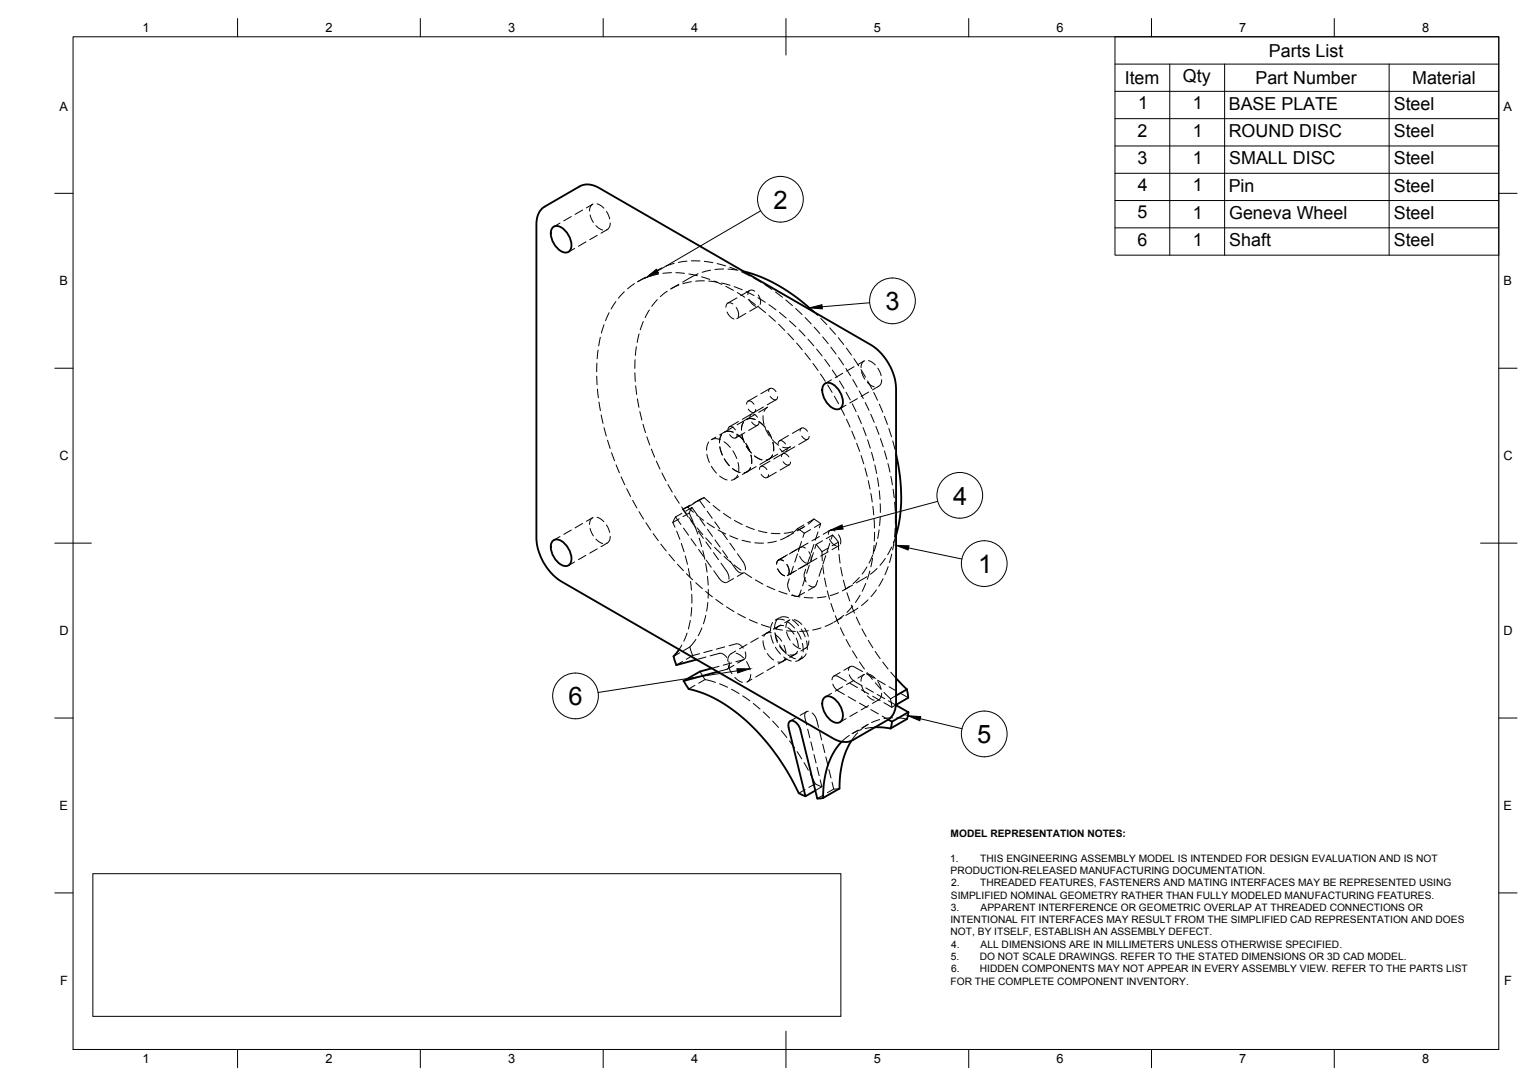
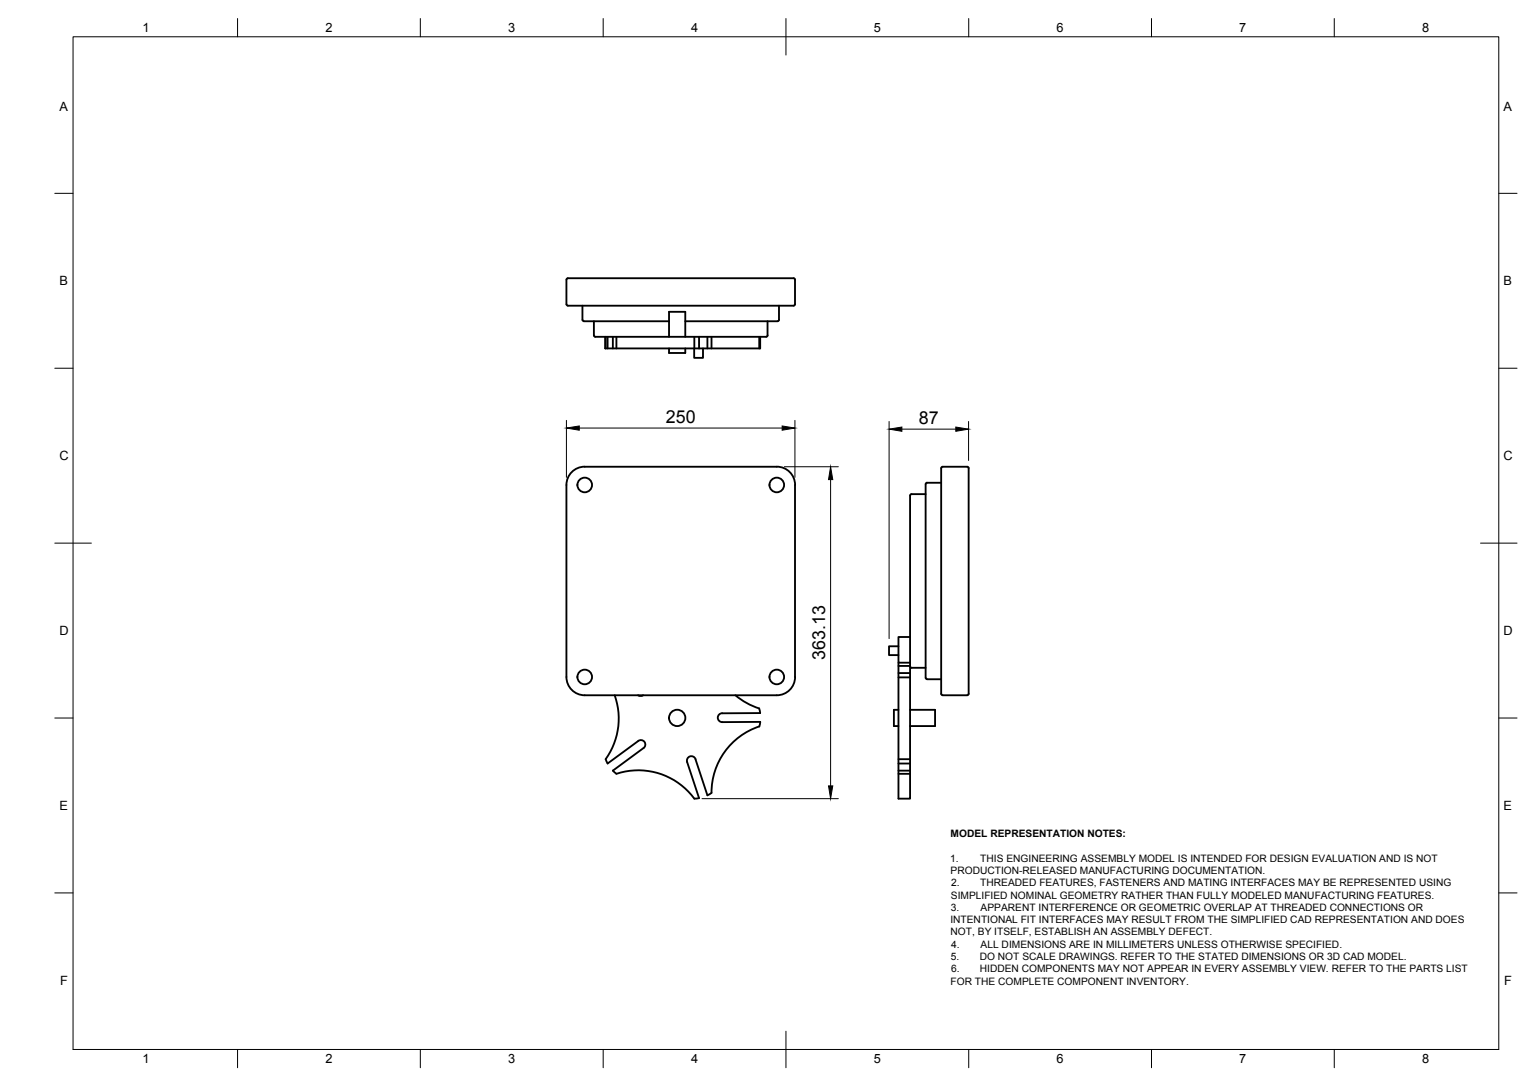
ISO-10303-21;
HEADER;
/* Generated by software containing ST-Developer
 * from STEP Tools, Inc. (www.steptools.com) 
 */

FILE_DESCRIPTION(
/* description */ ('STEP AP214'),
/* implementation_level */ '2;1');

FILE_NAME(
/* name */ 'MAS-609',
/* time_stamp */ '2026-10-06T11:20:11-07:00',
/* author */ (''),
/* organization */ (''),
/* preprocessor_version */ 'ST-DEVELOPER v20.2',
/* originating_system */ 'Autodesk Translation Framework v15.15.0.0',
/* authorisation */ '');

FILE_SCHEMA (('AUTOMOTIVE_DESIGN { 1 0 10303 214 3 1 1 }'));
ENDSEC;

DATA;
#10=MECHANICAL_DESIGN_GEOMETRIC_PRESENTATION_REPRESENTATION('',(#47,#48,
#49,#50,#51,#52),#2840);
#11=ITEM_DEFINED_TRANSFORMATION($,$,#1621,#1835);
#12=ITEM_DEFINED_TRANSFORMATION($,$,#1696,#1836);
#13=ITEM_DEFINED_TRANSFORMATION($,$,#1709,#1837);
#14=ITEM_DEFINED_TRANSFORMATION($,$,#1743,#1838);
#15=ITEM_DEFINED_TRANSFORMATION($,$,#1749,#1839);
#16=ITEM_DEFINED_TRANSFORMATION($,$,#1829,#1840);
#17=(
REPRESENTATION_RELATIONSHIP($,$,#2866,#2865)
REPRESENTATION_RELATIONSHIP_WITH_TRANSFORMATION(#11)
SHAPE_REPRESENTATION_RELATIONSHIP()
);
#18=(
REPRESENTATION_RELATIONSHIP($,$,#2867,#2865)
REPRESENTATION_RELATIONSHIP_WITH_TRANSFORMATION(#12)
SHAPE_REPRESENTATION_RELATIONSHIP()
);
#19=(
REPRESENTATION_RELATIONSHIP($,$,#2868,#2865)
REPRESENTATION_RELATIONSHIP_WITH_TRANSFORMATION(#13)
SHAPE_REPRESENTATION_RELATIONSHIP()
);
#20=(
REPRESENTATION_RELATIONSHIP($,$,#2869,#2865)
REPRESENTATION_RELATIONSHIP_WITH_TRANSFORMATION(#14)
SHAPE_REPRESENTATION_RELATIONSHIP()
);
#21=(
REPRESENTATION_RELATIONSHIP($,$,#2870,#2865)
REPRESENTATION_RELATIONSHIP_WITH_TRANSFORMATION(#15)
SHAPE_REPRESENTATION_RELATIONSHIP()
);
#22=(
REPRESENTATION_RELATIONSHIP($,$,#2871,#2865)
REPRESENTATION_RELATIONSHIP_WITH_TRANSFORMATION(#16)
SHAPE_REPRESENTATION_RELATIONSHIP()
);
#23=CONTEXT_DEPENDENT_SHAPE_REPRESENTATION(#17,#2859);
#24=CONTEXT_DEPENDENT_SHAPE_REPRESENTATION(#18,#2860);
#25=CONTEXT_DEPENDENT_SHAPE_REPRESENTATION(#19,#2861);
#26=CONTEXT_DEPENDENT_SHAPE_REPRESENTATION(#20,#2862);
#27=CONTEXT_DEPENDENT_SHAPE_REPRESENTATION(#21,#2863);
#28=CONTEXT_DEPENDENT_SHAPE_REPRESENTATION(#22,#2864);
#29=NEXT_ASSEMBLY_USAGE_OCCURRENCE('BASE PLATE:1','BASE PLATE:1',
'BASE PLATE:1',#2873,#2874,'BASE PLATE:1');
#30=NEXT_ASSEMBLY_USAGE_OCCURRENCE('ROUND DISC:1','ROUND DISC:1',
'ROUND DISC:1',#2873,#2875,'ROUND DISC:1');
#31=NEXT_ASSEMBLY_USAGE_OCCURRENCE('SMALL DISC:1','SMALL DISC:1',
'SMALL DISC:1',#2873,#2876,'SMALL DISC:1');
#32=NEXT_ASSEMBLY_USAGE_OCCURRENCE('PIN:1','PIN:1','PIN:1',#2873,#2877,
'PIN:1');
#33=NEXT_ASSEMBLY_USAGE_OCCURRENCE('Geneva Wheel:1','Geneva Wheel:1',
'Geneva Wheel:1',#2873,#2878,'Geneva Wheel:1');
#34=NEXT_ASSEMBLY_USAGE_OCCURRENCE('SHAFT:1','SHAFT:1','SHAFT:1',#2873,
#2879,'SHAFT:1');
#35=SHAPE_REPRESENTATION_RELATIONSHIP('SRR','None',#2866,#41);
#36=SHAPE_REPRESENTATION_RELATIONSHIP('SRR','None',#2867,#42);
#37=SHAPE_REPRESENTATION_RELATIONSHIP('SRR','None',#2868,#43);
#38=SHAPE_REPRESENTATION_RELATIONSHIP('SRR','None',#2869,#44);
#39=SHAPE_REPRESENTATION_RELATIONSHIP('SRR','None',#2870,#45);
#40=SHAPE_REPRESENTATION_RELATIONSHIP('SRR','None',#2871,#46);
#41=ADVANCED_BREP_SHAPE_REPRESENTATION('',(#53),#2834);
#42=ADVANCED_BREP_SHAPE_REPRESENTATION('',(#54),#2835);
#43=ADVANCED_BREP_SHAPE_REPRESENTATION('',(#55),#2836);
#44=ADVANCED_BREP_SHAPE_REPRESENTATION('',(#56),#2837);
#45=ADVANCED_BREP_SHAPE_REPRESENTATION('',(#57),#2838);
#46=ADVANCED_BREP_SHAPE_REPRESENTATION('',(#58),#2839);
#47=STYLED_ITEM('',(#2905),#53);
#48=STYLED_ITEM('',(#2905),#54);
#49=STYLED_ITEM('',(#2905),#55);
#50=STYLED_ITEM('',(#2905),#56);
#51=STYLED_ITEM('',(#2905),#57);
#52=STYLED_ITEM('',(#2905),#58);
#53=MANIFOLD_SOLID_BREP('Body1',#1547);
#54=MANIFOLD_SOLID_BREP('Body1',#1548);
#55=MANIFOLD_SOLID_BREP('Body1',#1549);
#56=MANIFOLD_SOLID_BREP('Body1',#1550);
#57=MANIFOLD_SOLID_BREP('Body1',#1551);
#58=MANIFOLD_SOLID_BREP('Body1',#1552);
#59=TOROIDAL_SURFACE('',#1663,18.5,1.5);
#60=TOROIDAL_SURFACE('',#1670,18.5,1.5);
#61=TOROIDAL_SURFACE('',#1672,18.5,1.5);
#62=TOROIDAL_SURFACE('',#1678,18.5,1.5);
#63=TOROIDAL_SURFACE('',#1679,18.5,1.5);
#64=TOROIDAL_SURFACE('',#1686,18.5,1.5);
#65=TOROIDAL_SURFACE('',#1688,18.5,1.5);
#66=TOROIDAL_SURFACE('',#1694,18.5,1.5);
#67=TOROIDAL_SURFACE('',#1700,106.,1.5);
#68=TOROIDAL_SURFACE('',#1728,13.,0.5);
#69=TOROIDAL_SURFACE('',#1734,93.5,1.5);
#70=FACE_BOUND('',#226,.T.);
#71=FACE_BOUND('',#227,.T.);
#72=FACE_BOUND('',#228,.T.);
#73=FACE_BOUND('',#229,.T.);
#74=FACE_BOUND('',#230,.T.);
#75=FACE_BOUND('',#232,.T.);
#76=FACE_BOUND('',#233,.T.);
#77=FACE_BOUND('',#234,.T.);
#78=FACE_BOUND('',#235,.T.);
#79=FACE_BOUND('',#261,.T.);
#80=FACE_BOUND('',#263,.T.);
#81=FACE_BOUND('',#275,.T.);
#82=FACE_BOUND('',#276,.T.);
#83=FACE_BOUND('',#277,.T.);
#84=FACE_BOUND('',#278,.T.);
#85=FACE_BOUND('',#279,.T.);
#86=FACE_BOUND('',#280,.T.);
#87=FACE_BOUND('',#281,.T.);
#88=FACE_BOUND('',#283,.T.);
#89=FACE_BOUND('',#284,.T.);
#90=FACE_BOUND('',#285,.T.);
#91=FACE_BOUND('',#286,.T.);
#92=FACE_BOUND('',#287,.T.);
#93=FACE_BOUND('',#288,.T.);
#94=FACE_BOUND('',#289,.T.);
#95=FACE_BOUND('',#299,.T.);
#96=FACE_BOUND('',#301,.T.);
#97=FACE_BOUND('',#330,.T.);
#98=PLANE('',#1637);
#99=PLANE('',#1638);
#100=PLANE('',#1639);
#101=PLANE('',#1640);
#102=PLANE('',#1641);
#103=PLANE('',#1646);
#104=PLANE('',#1695);
#105=PLANE('',#1707);
#106=PLANE('',#1708);
#107=PLANE('',#1741);
#108=PLANE('',#1742);
#109=PLANE('',#1747);
#110=PLANE('',#1748);
#111=PLANE('',#1765);
#112=PLANE('',#1783);
#113=PLANE('',#1802);
#114=PLANE('',#1806);
#115=PLANE('',#1808);
#116=PLANE('',#1812);
#117=PLANE('',#1813);
#118=PLANE('',#1816);
#119=PLANE('',#1817);
#120=PLANE('',#1821);
#121=PLANE('',#1823);
#122=PLANE('',#1827);
#123=PLANE('',#1828);
#124=PLANE('',#1833);
#125=PLANE('',#1834);
#126=FACE_OUTER_BOUND('',#216,.T.);
#127=FACE_OUTER_BOUND('',#217,.T.);
#128=FACE_OUTER_BOUND('',#218,.T.);
#129=FACE_OUTER_BOUND('',#219,.T.);
#130=FACE_OUTER_BOUND('',#220,.T.);
#131=FACE_OUTER_BOUND('',#221,.T.);
#132=FACE_OUTER_BOUND('',#222,.T.);
#133=FACE_OUTER_BOUND('',#223,.T.);
#134=FACE_OUTER_BOUND('',#224,.T.);
#135=FACE_OUTER_BOUND('',#225,.T.);
#136=FACE_OUTER_BOUND('',#231,.T.);
#137=FACE_OUTER_BOUND('',#236,.T.);
#138=FACE_OUTER_BOUND('',#237,.T.);
#139=FACE_OUTER_BOUND('',#238,.T.);
#140=FACE_OUTER_BOUND('',#239,.T.);
#141=FACE_OUTER_BOUND('',#240,.T.);
#142=FACE_OUTER_BOUND('',#241,.T.);
#143=FACE_OUTER_BOUND('',#242,.T.);
#144=FACE_OUTER_BOUND('',#243,.T.);
#145=FACE_OUTER_BOUND('',#244,.T.);
#146=FACE_OUTER_BOUND('',#245,.T.);
#147=FACE_OUTER_BOUND('',#246,.T.);
#148=FACE_OUTER_BOUND('',#247,.T.);
#149=FACE_OUTER_BOUND('',#248,.T.);
#150=FACE_OUTER_BOUND('',#249,.T.);
#151=FACE_OUTER_BOUND('',#250,.T.);
#152=FACE_OUTER_BOUND('',#251,.T.);
#153=FACE_OUTER_BOUND('',#252,.T.);
#154=FACE_OUTER_BOUND('',#253,.T.);
#155=FACE_OUTER_BOUND('',#254,.T.);
#156=FACE_OUTER_BOUND('',#255,.T.);
#157=FACE_OUTER_BOUND('',#256,.T.);
#158=FACE_OUTER_BOUND('',#257,.T.);
#159=FACE_OUTER_BOUND('',#258,.T.);
#160=FACE_OUTER_BOUND('',#259,.T.);
#161=FACE_OUTER_BOUND('',#260,.T.);
#162=FACE_OUTER_BOUND('',#262,.T.);
#163=FACE_OUTER_BOUND('',#264,.T.);
#164=FACE_OUTER_BOUND('',#265,.T.);
#165=FACE_OUTER_BOUND('',#266,.T.);
#166=FACE_OUTER_BOUND('',#267,.T.);
#167=FACE_OUTER_BOUND('',#268,.T.);
#168=FACE_OUTER_BOUND('',#269,.T.);
#169=FACE_OUTER_BOUND('',#270,.T.);
#170=FACE_OUTER_BOUND('',#271,.T.);
#171=FACE_OUTER_BOUND('',#272,.T.);
#172=FACE_OUTER_BOUND('',#273,.T.);
#173=FACE_OUTER_BOUND('',#274,.T.);
#174=FACE_OUTER_BOUND('',#282,.T.);
#175=FACE_OUTER_BOUND('',#290,.T.);
#176=FACE_OUTER_BOUND('',#291,.T.);
#177=FACE_OUTER_BOUND('',#292,.T.);
#178=FACE_OUTER_BOUND('',#293,.T.);
#179=FACE_OUTER_BOUND('',#294,.T.);
#180=FACE_OUTER_BOUND('',#295,.T.);
#181=FACE_OUTER_BOUND('',#296,.T.);
#182=FACE_OUTER_BOUND('',#297,.T.);
#183=FACE_OUTER_BOUND('',#298,.T.);
#184=FACE_OUTER_BOUND('',#300,.T.);
#185=FACE_OUTER_BOUND('',#302,.T.);
#186=FACE_OUTER_BOUND('',#303,.T.);
#187=FACE_OUTER_BOUND('',#304,.T.);
#188=FACE_OUTER_BOUND('',#305,.T.);
#189=FACE_OUTER_BOUND('',#306,.T.);
#190=FACE_OUTER_BOUND('',#307,.T.);
#191=FACE_OUTER_BOUND('',#308,.T.);
#192=FACE_OUTER_BOUND('',#309,.T.);
#193=FACE_OUTER_BOUND('',#310,.T.);
#194=FACE_OUTER_BOUND('',#311,.T.);
#195=FACE_OUTER_BOUND('',#312,.T.);
#196=FACE_OUTER_BOUND('',#313,.T.);
#197=FACE_OUTER_BOUND('',#314,.T.);
#198=FACE_OUTER_BOUND('',#315,.T.);
#199=FACE_OUTER_BOUND('',#316,.T.);
#200=FACE_OUTER_BOUND('',#317,.T.);
#201=FACE_OUTER_BOUND('',#318,.T.);
#202=FACE_OUTER_BOUND('',#319,.T.);
#203=FACE_OUTER_BOUND('',#320,.T.);
#204=FACE_OUTER_BOUND('',#321,.T.);
#205=FACE_OUTER_BOUND('',#322,.T.);
#206=FACE_OUTER_BOUND('',#323,.T.);
#207=FACE_OUTER_BOUND('',#324,.T.);
#208=FACE_OUTER_BOUND('',#325,.T.);
#209=FACE_OUTER_BOUND('',#326,.T.);
#210=FACE_OUTER_BOUND('',#327,.T.);
#211=FACE_OUTER_BOUND('',#328,.T.);
#212=FACE_OUTER_BOUND('',#329,.T.);
#213=FACE_OUTER_BOUND('',#331,.T.);
#214=FACE_OUTER_BOUND('',#332,.T.);
#215=FACE_OUTER_BOUND('',#333,.T.);
#216=EDGE_LOOP('',(#984,#985,#986,#987));
#217=EDGE_LOOP('',(#988,#989,#990,#991));
#218=EDGE_LOOP('',(#992,#993,#994,#995));
#219=EDGE_LOOP('',(#996,#997,#998,#999));
#220=EDGE_LOOP('',(#1000,#1001,#1002,#1003));
#221=EDGE_LOOP('',(#1004,#1005,#1006,#1007));
#222=EDGE_LOOP('',(#1008,#1009,#1010,#1011));
#223=EDGE_LOOP('',(#1012,#1013,#1014,#1015));
#224=EDGE_LOOP('',(#1016,#1017,#1018,#1019));
#225=EDGE_LOOP('',(#1020,#1021,#1022,#1023,#1024,#1025,#1026,#1027));
#226=EDGE_LOOP('',(#1028));
#227=EDGE_LOOP('',(#1029));
#228=EDGE_LOOP('',(#1030));
#229=EDGE_LOOP('',(#1031));
#230=EDGE_LOOP('',(#1032));
#231=EDGE_LOOP('',(#1033,#1034,#1035,#1036,#1037,#1038,#1039,#1040));
#232=EDGE_LOOP('',(#1041));
#233=EDGE_LOOP('',(#1042));
#234=EDGE_LOOP('',(#1043));
#235=EDGE_LOOP('',(#1044));
#236=EDGE_LOOP('',(#1045,#1046,#1047,#1048));
#237=EDGE_LOOP('',(#1049,#1050,#1051,#1052));
#238=EDGE_LOOP('',(#1053,#1054,#1055,#1056));
#239=EDGE_LOOP('',(#1057,#1058,#1059,#1060));
#240=EDGE_LOOP('',(#1061,#1062,#1063,#1064));
#241=EDGE_LOOP('',(#1065,#1066,#1067,#1068));
#242=EDGE_LOOP('',(#1069,#1070,#1071,#1072));
#243=EDGE_LOOP('',(#1073,#1074,#1075,#1076));
#244=EDGE_LOOP('',(#1077,#1078,#1079,#1080));
#245=EDGE_LOOP('',(#1081,#1082,#1083,#1084));
#246=EDGE_LOOP('',(#1085,#1086,#1087,#1088));
#247=EDGE_LOOP('',(#1089,#1090,#1091,#1092));
#248=EDGE_LOOP('',(#1093,#1094,#1095,#1096));
#249=EDGE_LOOP('',(#1097,#1098,#1099,#1100));
#250=EDGE_LOOP('',(#1101,#1102,#1103,#1104));
#251=EDGE_LOOP('',(#1105,#1106,#1107,#1108));
#252=EDGE_LOOP('',(#1109,#1110,#1111,#1112));
#253=EDGE_LOOP('',(#1113,#1114,#1115,#1116));
#254=EDGE_LOOP('',(#1117,#1118,#1119,#1120));
#255=EDGE_LOOP('',(#1121,#1122,#1123,#1124));
#256=EDGE_LOOP('',(#1125));
#257=EDGE_LOOP('',(#1126,#1127,#1128,#1129));
#258=EDGE_LOOP('',(#1130,#1131,#1132,#1133,#1134));
#259=EDGE_LOOP('',(#1135,#1136,#1137,#1138,#1139));
#260=EDGE_LOOP('',(#1140));
#261=EDGE_LOOP('',(#1141));
#262=EDGE_LOOP('',(#1142));
#263=EDGE_LOOP('',(#1143));
#264=EDGE_LOOP('',(#1144,#1145,#1146,#1147));
#265=EDGE_LOOP('',(#1148,#1149,#1150,#1151));
#266=EDGE_LOOP('',(#1152,#1153,#1154,#1155));
#267=EDGE_LOOP('',(#1156,#1157,#1158,#1159));
#268=EDGE_LOOP('',(#1160,#1161,#1162,#1163));
#269=EDGE_LOOP('',(#1164,#1165,#1166,#1167));
#270=EDGE_LOOP('',(#1168,#1169,#1170,#1171));
#271=EDGE_LOOP('',(#1172,#1173,#1174,#1175));
#272=EDGE_LOOP('',(#1176,#1177,#1178,#1179,#1180));
#273=EDGE_LOOP('',(#1181,#1182,#1183,#1184,#1185));
#274=EDGE_LOOP('',(#1186));
#275=EDGE_LOOP('',(#1187));
#276=EDGE_LOOP('',(#1188));
#277=EDGE_LOOP('',(#1189));
#278=EDGE_LOOP('',(#1190));
#279=EDGE_LOOP('',(#1191));
#280=EDGE_LOOP('',(#1192));
#281=EDGE_LOOP('',(#1193));
#282=EDGE_LOOP('',(#1194));
#283=EDGE_LOOP('',(#1195));
#284=EDGE_LOOP('',(#1196));
#285=EDGE_LOOP('',(#1197));
#286=EDGE_LOOP('',(#1198));
#287=EDGE_LOOP('',(#1199));
#288=EDGE_LOOP('',(#1200));
#289=EDGE_LOOP('',(#1201));
#290=EDGE_LOOP('',(#1202,#1203,#1204,#1205));
#291=EDGE_LOOP('',(#1206));
#292=EDGE_LOOP('',(#1207));
#293=EDGE_LOOP('',(#1208,#1209,#1210,#1211));
#294=EDGE_LOOP('',(#1212,#1213,#1214,#1215));
#295=EDGE_LOOP('',(#1216,#1217,#1218,#1219));
#296=EDGE_LOOP('',(#1220,#1221,#1222,#1223));
#297=EDGE_LOOP('',(#1224,#1225,#1226,#1227));
#298=EDGE_LOOP('',(#1228,#1229,#1230,#1231,#1232,#1233,#1234,#1235,#1236,
#1237,#1238,#1239,#1240,#1241,#1242,#1243,#1244,#1245,#1246,#1247,#1248,
#1249,#1250,#1251,#1252,#1253,#1254,#1255,#1256,#1257));
#299=EDGE_LOOP('',(#1258));
#300=EDGE_LOOP('',(#1259,#1260,#1261,#1262,#1263,#1264,#1265,#1266,#1267,
#1268,#1269,#1270,#1271,#1272,#1273,#1274,#1275,#1276,#1277,#1278,#1279,
#1280,#1281,#1282,#1283,#1284,#1285,#1286,#1287,#1288));
#301=EDGE_LOOP('',(#1289));
#302=EDGE_LOOP('',(#1290,#1291,#1292,#1293));
#303=EDGE_LOOP('',(#1294,#1295,#1296,#1297));
#304=EDGE_LOOP('',(#1298,#1299,#1300,#1301));
#305=EDGE_LOOP('',(#1302,#1303,#1304,#1305));
#306=EDGE_LOOP('',(#1306,#1307,#1308,#1309));
#307=EDGE_LOOP('',(#1310,#1311,#1312,#1313));
#308=EDGE_LOOP('',(#1314,#1315,#1316,#1317));
#309=EDGE_LOOP('',(#1318,#1319,#1320,#1321));
#310=EDGE_LOOP('',(#1322,#1323,#1324,#1325));
#311=EDGE_LOOP('',(#1326,#1327,#1328,#1329));
#312=EDGE_LOOP('',(#1330,#1331,#1332,#1333));
#313=EDGE_LOOP('',(#1334,#1335,#1336,#1337));
#314=EDGE_LOOP('',(#1338,#1339,#1340,#1341));
#315=EDGE_LOOP('',(#1342,#1343,#1344,#1345));
#316=EDGE_LOOP('',(#1346,#1347,#1348,#1349));
#317=EDGE_LOOP('',(#1350,#1351,#1352,#1353));
#318=EDGE_LOOP('',(#1354,#1355,#1356,#1357));
#319=EDGE_LOOP('',(#1358,#1359,#1360,#1361));
#320=EDGE_LOOP('',(#1362,#1363,#1364,#1365));
#321=EDGE_LOOP('',(#1366,#1367,#1368,#1369));
#322=EDGE_LOOP('',(#1370,#1371,#1372,#1373));
#323=EDGE_LOOP('',(#1374,#1375,#1376,#1377));
#324=EDGE_LOOP('',(#1378,#1379,#1380,#1381));
#325=EDGE_LOOP('',(#1382,#1383,#1384,#1385));
#326=EDGE_LOOP('',(#1386,#1387,#1388,#1389));
#327=EDGE_LOOP('',(#1390,#1391,#1392,#1393));
#328=EDGE_LOOP('',(#1394,#1395,#1396,#1397));
#329=EDGE_LOOP('',(#1398));
#330=EDGE_LOOP('',(#1399));
#331=EDGE_LOOP('',(#1400,#1401,#1402,#1403));
#332=EDGE_LOOP('',(#1404));
#333=EDGE_LOOP('',(#1405));
#334=LINE('',#2382,#427);
#335=LINE('',#2388,#428);
#336=LINE('',#2394,#429);
#337=LINE('',#2400,#430);
#338=LINE('',#2406,#431);
#339=LINE('',#2411,#432);
#340=LINE('',#2413,#433);
#341=LINE('',#2415,#434);
#342=LINE('',#2416,#435);
#343=LINE('',#2420,#436);
#344=LINE('',#2422,#437);
#345=LINE('',#2424,#438);
#346=LINE('',#2425,#439);
#347=LINE('',#2429,#440);
#348=LINE('',#2431,#441);
#349=LINE('',#2433,#442);
#350=LINE('',#2434,#443);
#351=LINE('',#2438,#444);
#352=LINE('',#2440,#445);
#353=LINE('',#2442,#446);
#354=LINE('',#2443,#447);
#355=LINE('',#2447,#448);
#356=LINE('',#2451,#449);
#357=LINE('',#2455,#450);
#358=LINE('',#2459,#451);
#359=LINE('',#2464,#452);
#360=LINE('',#2468,#453);
#361=LINE('',#2472,#454);
#362=LINE('',#2476,#455);
#363=LINE('',#2528,#456);
#364=LINE('',#2541,#457);
#365=LINE('',#2549,#458);
#366=LINE('',#2555,#459);
#367=LINE('',#2561,#460);
#368=LINE('',#2567,#461);
#369=LINE('',#2573,#462);
#370=LINE('',#2579,#463);
#371=LINE('',#2590,#464);
#372=LINE('',#2602,#465);
#373=LINE('',#2610,#466);
#374=LINE('',#2619,#467);
#375=LINE('',#2626,#468);
#376=LINE('',#2629,#469);
#377=LINE('',#2635,#470);
#378=LINE('',#2638,#471);
#379=LINE('',#2644,#472);
#380=LINE('',#2647,#473);
#381=LINE('',#2652,#474);
#382=LINE('',#2659,#475);
#383=LINE('',#2667,#476);
#384=LINE('',#2671,#477);
#385=LINE('',#2678,#478);
#386=LINE('',#2680,#479);
#387=LINE('',#2684,#480);
#388=LINE('',#2686,#481);
#389=LINE('',#2694,#482);
#390=LINE('',#2698,#483);
#391=LINE('',#2705,#484);
#392=LINE('',#2711,#485);
#393=LINE('',#2719,#486);
#394=LINE('',#2723,#487);
#395=LINE('',#2730,#488);
#396=LINE('',#2732,#489);
#397=LINE('',#2736,#490);
#398=LINE('',#2738,#491);
#399=LINE('',#2746,#492);
#400=LINE('',#2750,#493);
#401=LINE('',#2757,#494);
#402=LINE('',#2759,#495);
#403=LINE('',#2760,#496);
#404=LINE('',#2762,#497);
#405=LINE('',#2764,#498);
#406=LINE('',#2766,#499);
#407=LINE('',#2768,#500);
#408=LINE('',#2770,#501);
#409=LINE('',#2772,#502);
#410=LINE('',#2774,#503);
#411=LINE('',#2776,#504);
#412=LINE('',#2778,#505);
#413=LINE('',#2780,#506);
#414=LINE('',#2783,#507);
#415=LINE('',#2786,#508);
#416=LINE('',#2789,#509);
#417=LINE('',#2791,#510);
#418=LINE('',#2793,#511);
#419=LINE('',#2795,#512);
#420=LINE('',#2797,#513);
#421=LINE('',#2799,#514);
#422=LINE('',#2801,#515);
#423=LINE('',#2803,#516);
#424=LINE('',#2805,#517);
#425=LINE('',#2807,#518);
#426=LINE('',#2815,#519);
#427=VECTOR('',#1849,12.5000000000002);
#428=VECTOR('',#1856,8.00000000000001);
#429=VECTOR('',#1863,8.00000000000001);
#430=VECTOR('',#1870,8.00000000000001);
#431=VECTOR('',#1877,8.00000000000001);
#432=VECTOR('',#1882,1000.);
#433=VECTOR('',#1883,1000.);
#434=VECTOR('',#1884,1000.);
#435=VECTOR('',#1885,1000.);
#436=VECTOR('',#1888,1000.);
#437=VECTOR('',#1889,1000.);
#438=VECTOR('',#1890,1000.);
#439=VECTOR('',#1891,1000.);
#440=VECTOR('',#1894,1000.);
#441=VECTOR('',#1895,1000.);
#442=VECTOR('',#1896,1000.);
#443=VECTOR('',#1897,1000.);
#444=VECTOR('',#1900,1000.);
#445=VECTOR('',#1901,1000.);
#446=VECTOR('',#1902,1000.);
#447=VECTOR('',#1903,1000.);
#448=VECTOR('',#1906,1000.);
#449=VECTOR('',#1909,1000.);
#450=VECTOR('',#1912,1000.);
#451=VECTOR('',#1915,1000.);
#452=VECTOR('',#1920,1000.);
#453=VECTOR('',#1923,1000.);
#454=VECTOR('',#1926,1000.);
#455=VECTOR('',#1929,1000.);
#456=VECTOR('',#2028,12.5);
#457=VECTOR('',#2045,107.5);
#458=VECTOR('',#2056,4.92500000000001);
#459=VECTOR('',#2063,4.92500000000001);
#460=VECTOR('',#2070,3.5);
#461=VECTOR('',#2077,3.5);
#462=VECTOR('',#2084,3.5);
#463=VECTOR('',#2091,3.5);
#464=VECTOR('',#2106,12.5);
#465=VECTOR('',#2121,95.0000000000003);
#466=VECTOR('',#2132,4.83000000000002);
#467=VECTOR('',#2145,12.7);
#468=VECTOR('',#2152,1000.);
#469=VECTOR('',#2155,1000.);
#470=VECTOR('',#2160,1000.);
#471=VECTOR('',#2163,1000.);
#472=VECTOR('',#2168,1000.);
#473=VECTOR('',#2171,1000.);
#474=VECTOR('',#2176,8.88999999999999);
#475=VECTOR('',#2183,1000.);
#476=VECTOR('',#2190,1000.);
#477=VECTOR('',#2193,1000.);
#478=VECTOR('',#2200,1000.);
#479=VECTOR('',#2201,1000.);
#480=VECTOR('',#2206,1000.);
#481=VECTOR('',#2207,1000.);
#482=VECTOR('',#2214,1000.);
#483=VECTOR('',#2217,1000.);
#484=VECTOR('',#2224,1000.);
#485=VECTOR('',#2229,1000.);
#486=VECTOR('',#2236,1000.);
#487=VECTOR('',#2239,1000.);
#488=VECTOR('',#2246,1000.);
#489=VECTOR('',#2247,1000.);
#490=VECTOR('',#2252,1000.);
#491=VECTOR('',#2253,1000.);
#492=VECTOR('',#2260,1000.);
#493=VECTOR('',#2263,1000.);
#494=VECTOR('',#2270,1000.);
#495=VECTOR('',#2273,1000.);
#496=VECTOR('',#2274,1000.);
#497=VECTOR('',#2277,1000.);
#498=VECTOR('',#2280,1000.);
#499=VECTOR('',#2283,1000.);
#500=VECTOR('',#2286,1000.);
#501=VECTOR('',#2289,1000.);
#502=VECTOR('',#2292,1000.);
#503=VECTOR('',#2295,1000.);
#504=VECTOR('',#2298,1000.);
#505=VECTOR('',#2301,1000.);
#506=VECTOR('',#2304,1000.);
#507=VECTOR('',#2309,1000.);
#508=VECTOR('',#2314,1000.);
#509=VECTOR('',#2319,1000.);
#510=VECTOR('',#2322,1000.);
#511=VECTOR('',#2325,1000.);
#512=VECTOR('',#2328,1000.);
#513=VECTOR('',#2331,1000.);
#514=VECTOR('',#2334,1000.);
#515=VECTOR('',#2337,1000.);
#516=VECTOR('',#2340,1000.);
#517=VECTOR('',#2343,1000.);
#518=VECTOR('',#2346,1000.);
#519=VECTOR('',#2357,8.89);
#520=CIRCLE('',#1623,12.5000000000002);
#521=CIRCLE('',#1624,12.5000000000002);
#522=CIRCLE('',#1626,8.00000000000001);
#523=CIRCLE('',#1627,8.00000000000001);
#524=CIRCLE('',#1629,8.00000000000001);
#525=CIRCLE('',#1630,8.00000000000001);
#526=CIRCLE('',#1632,8.00000000000001);
#527=CIRCLE('',#1633,8.00000000000001);
#528=CIRCLE('',#1635,8.00000000000001);
#529=CIRCLE('',#1636,8.00000000000001);
#530=CIRCLE('',#1642,18.5);
#531=CIRCLE('',#1643,18.5);
#532=CIRCLE('',#1644,18.5);
#533=CIRCLE('',#1645,18.5);
#534=CIRCLE('',#1647,18.5);
#535=CIRCLE('',#1648,18.5);
#536=CIRCLE('',#1649,18.5);
#537=CIRCLE('',#1650,18.5);
#538=CIRCLE('',#1652,20.);
#539=CIRCLE('',#1653,20.);
#540=CIRCLE('',#1655,20.);
#541=CIRCLE('',#1656,20.);
#542=CIRCLE('',#1658,20.);
#543=CIRCLE('',#1659,20.);
#544=CIRCLE('',#1661,20.);
#545=CIRCLE('',#1662,20.);
#546=CIRCLE('',#1664,1.5);
#547=CIRCLE('',#1665,1.50000000000006);
#548=CIRCLE('',#1667,1.50000000000006);
#549=CIRCLE('',#1669,1.5);
#550=CIRCLE('',#1671,1.5);
#551=CIRCLE('',#1673,1.50000000000006);
#552=CIRCLE('',#1675,1.5);
#553=CIRCLE('',#1677,1.50000000000006);
#554=CIRCLE('',#1680,1.5);
#555=CIRCLE('',#1681,1.50000000000006);
#556=CIRCLE('',#1683,1.50000000000006);
#557=CIRCLE('',#1685,1.5);
#558=CIRCLE('',#1687,1.5);
#559=CIRCLE('',#1689,1.50000000000006);
#560=CIRCLE('',#1691,1.5);
#561=CIRCLE('',#1693,1.50000000000006);
#562=CIRCLE('',#1698,12.5);
#563=CIRCLE('',#1699,12.5);
#564=CIRCLE('',#1701,106.);
#565=CIRCLE('',#1702,1.5);
#566=CIRCLE('',#1703,107.5);
#567=CIRCLE('',#1704,107.5);
#568=CIRCLE('',#1706,107.5);
#569=CIRCLE('',#1711,4.92500000000001);
#570=CIRCLE('',#1712,4.92500000000001);
#571=CIRCLE('',#1714,4.92500000000001);
#572=CIRCLE('',#1715,4.92500000000001);
#573=CIRCLE('',#1717,3.5);
#574=CIRCLE('',#1718,3.5);
#575=CIRCLE('',#1720,3.5);
#576=CIRCLE('',#1721,3.5);
#577=CIRCLE('',#1723,3.5);
#578=CIRCLE('',#1724,3.5);
#579=CIRCLE('',#1726,3.5);
#580=CIRCLE('',#1727,3.5);
#581=CIRCLE('',#1729,12.5000000000001);
#582=CIRCLE('',#1730,0.5);
#583=CIRCLE('',#1731,13.0000000000001);
#584=CIRCLE('',#1733,12.5000000000001);
#585=CIRCLE('',#1735,93.5000000000003);
#586=CIRCLE('',#1736,1.5);
#587=CIRCLE('',#1737,95.0000000000003);
#588=CIRCLE('',#1738,95.0000000000003);
#589=CIRCLE('',#1740,95.0000000000003);
#590=CIRCLE('',#1745,4.83000000000002);
#591=CIRCLE('',#1746,4.83000000000002);
#592=CIRCLE('',#1751,12.7);
#593=CIRCLE('',#1752,12.7);
#594=CIRCLE('',#1754,4.826);
#595=CIRCLE('',#1755,4.826);
#596=CIRCLE('',#1757,76.1999999999999);
#597=CIRCLE('',#1758,76.1999999999999);
#598=CIRCLE('',#1760,4.826);
#599=CIRCLE('',#1761,4.826);
#600=CIRCLE('',#1763,8.88999999999999);
#601=CIRCLE('',#1764,8.88999999999999);
#602=CIRCLE('',#1766,4.826);
#603=CIRCLE('',#1767,27.0465001077289);
#604=CIRCLE('',#1768,76.2);
#605=CIRCLE('',#1769,27.0465001077289);
#606=CIRCLE('',#1770,4.826);
#607=CIRCLE('',#1771,27.0465001077289);
#608=CIRCLE('',#1772,76.1999999999999);
#609=CIRCLE('',#1773,27.0465001077289);
#610=CIRCLE('',#1774,27.0465001077289);
#611=CIRCLE('',#1775,27.0465001077289);
#612=CIRCLE('',#1776,27.0465001077289);
#613=CIRCLE('',#1777,76.1999999999999);
#614=CIRCLE('',#1778,27.0465001077289);
#615=CIRCLE('',#1779,4.826);
#616=CIRCLE('',#1780,27.0465001077289);
#617=CIRCLE('',#1781,76.1999999999999);
#618=CIRCLE('',#1782,27.0465001077289);
#619=CIRCLE('',#1784,4.826);
#620=CIRCLE('',#1785,27.0465001077289);
#621=CIRCLE('',#1786,76.1999999999999);
#622=CIRCLE('',#1787,27.0465001077289);
#623=CIRCLE('',#1788,4.826);
#624=CIRCLE('',#1789,27.0465001077289);
#625=CIRCLE('',#1790,76.1999999999999);
#626=CIRCLE('',#1791,27.0465001077289);
#627=CIRCLE('',#1792,27.0465001077289);
#628=CIRCLE('',#1793,27.0465001077289);
#629=CIRCLE('',#1794,27.0465001077289);
#630=CIRCLE('',#1795,76.1999999999999);
#631=CIRCLE('',#1796,27.0465001077289);
#632=CIRCLE('',#1797,4.826);
#633=CIRCLE('',#1798,27.0465001077289);
#634=CIRCLE('',#1799,76.2);
#635=CIRCLE('',#1800,27.0465001077289);
#636=CIRCLE('',#1831,8.89);
#637=CIRCLE('',#1832,8.89);
#638=VERTEX_POINT('',#2379);
#639=VERTEX_POINT('',#2381);
#640=VERTEX_POINT('',#2385);
#641=VERTEX_POINT('',#2387);
#642=VERTEX_POINT('',#2391);
#643=VERTEX_POINT('',#2393);
#644=VERTEX_POINT('',#2397);
#645=VERTEX_POINT('',#2399);
#646=VERTEX_POINT('',#2403);
#647=VERTEX_POINT('',#2405);
#648=VERTEX_POINT('',#2409);
#649=VERTEX_POINT('',#2410);
#650=VERTEX_POINT('',#2412);
#651=VERTEX_POINT('',#2414);
#652=VERTEX_POINT('',#2418);
#653=VERTEX_POINT('',#2419);
#654=VERTEX_POINT('',#2421);
#655=VERTEX_POINT('',#2423);
#656=VERTEX_POINT('',#2427);
#657=VERTEX_POINT('',#2428);
#658=VERTEX_POINT('',#2430);
#659=VERTEX_POINT('',#2432);
#660=VERTEX_POINT('',#2436);
#661=VERTEX_POINT('',#2437);
#662=VERTEX_POINT('',#2439);
#663=VERTEX_POINT('',#2441);
#664=VERTEX_POINT('',#2445);
#665=VERTEX_POINT('',#2446);
#666=VERTEX_POINT('',#2448);
#667=VERTEX_POINT('',#2450);
#668=VERTEX_POINT('',#2452);
#669=VERTEX_POINT('',#2454);
#670=VERTEX_POINT('',#2456);
#671=VERTEX_POINT('',#2458);
#672=VERTEX_POINT('',#2462);
#673=VERTEX_POINT('',#2463);
#674=VERTEX_POINT('',#2465);
#675=VERTEX_POINT('',#2467);
#676=VERTEX_POINT('',#2469);
#677=VERTEX_POINT('',#2471);
#678=VERTEX_POINT('',#2473);
#679=VERTEX_POINT('',#2475);
#680=VERTEX_POINT('',#2525);
#681=VERTEX_POINT('',#2527);
#682=VERTEX_POINT('',#2531);
#683=VERTEX_POINT('',#2533);
#684=VERTEX_POINT('',#2535);
#685=VERTEX_POINT('',#2539);
#686=VERTEX_POINT('',#2546);
#687=VERTEX_POINT('',#2548);
#688=VERTEX_POINT('',#2552);
#689=VERTEX_POINT('',#2554);
#690=VERTEX_POINT('',#2558);
#691=VERTEX_POINT('',#2560);
#692=VERTEX_POINT('',#2564);
#693=VERTEX_POINT('',#2566);
#694=VERTEX_POINT('',#2570);
#695=VERTEX_POINT('',#2572);
#696=VERTEX_POINT('',#2576);
#697=VERTEX_POINT('',#2578);
#698=VERTEX_POINT('',#2582);
#699=VERTEX_POINT('',#2584);
#700=VERTEX_POINT('',#2588);
#701=VERTEX_POINT('',#2592);
#702=VERTEX_POINT('',#2594);
#703=VERTEX_POINT('',#2596);
#704=VERTEX_POINT('',#2600);
#705=VERTEX_POINT('',#2607);
#706=VERTEX_POINT('',#2609);
#707=VERTEX_POINT('',#2616);
#708=VERTEX_POINT('',#2618);
#709=VERTEX_POINT('',#2622);
#710=VERTEX_POINT('',#2623);
#711=VERTEX_POINT('',#2625);
#712=VERTEX_POINT('',#2627);
#713=VERTEX_POINT('',#2631);
#714=VERTEX_POINT('',#2632);
#715=VERTEX_POINT('',#2634);
#716=VERTEX_POINT('',#2636);
#717=VERTEX_POINT('',#2640);
#718=VERTEX_POINT('',#2641);
#719=VERTEX_POINT('',#2643);
#720=VERTEX_POINT('',#2645);
#721=VERTEX_POINT('',#2649);
#722=VERTEX_POINT('',#2651);
#723=VERTEX_POINT('',#2655);
#724=VERTEX_POINT('',#2656);
#725=VERTEX_POINT('',#2658);
#726=VERTEX_POINT('',#2660);
#727=VERTEX_POINT('',#2662);
#728=VERTEX_POINT('',#2664);
#729=VERTEX_POINT('',#2666);
#730=VERTEX_POINT('',#2668);
#731=VERTEX_POINT('',#2670);
#732=VERTEX_POINT('',#2672);
#733=VERTEX_POINT('',#2674);
#734=VERTEX_POINT('',#2676);
#735=VERTEX_POINT('',#2679);
#736=VERTEX_POINT('',#2682);
#737=VERTEX_POINT('',#2685);
#738=VERTEX_POINT('',#2687);
#739=VERTEX_POINT('',#2689);
#740=VERTEX_POINT('',#2691);
#741=VERTEX_POINT('',#2693);
#742=VERTEX_POINT('',#2695);
#743=VERTEX_POINT('',#2697);
#744=VERTEX_POINT('',#2699);
#745=VERTEX_POINT('',#2701);
#746=VERTEX_POINT('',#2703);
#747=VERTEX_POINT('',#2707);
#748=VERTEX_POINT('',#2708);
#749=VERTEX_POINT('',#2710);
#750=VERTEX_POINT('',#2712);
#751=VERTEX_POINT('',#2714);
#752=VERTEX_POINT('',#2716);
#753=VERTEX_POINT('',#2718);
#754=VERTEX_POINT('',#2720);
#755=VERTEX_POINT('',#2722);
#756=VERTEX_POINT('',#2724);
#757=VERTEX_POINT('',#2726);
#758=VERTEX_POINT('',#2728);
#759=VERTEX_POINT('',#2731);
#760=VERTEX_POINT('',#2734);
#761=VERTEX_POINT('',#2737);
#762=VERTEX_POINT('',#2739);
#763=VERTEX_POINT('',#2741);
#764=VERTEX_POINT('',#2743);
#765=VERTEX_POINT('',#2745);
#766=VERTEX_POINT('',#2747);
#767=VERTEX_POINT('',#2749);
#768=VERTEX_POINT('',#2751);
#769=VERTEX_POINT('',#2753);
#770=VERTEX_POINT('',#2755);
#771=VERTEX_POINT('',#2812);
#772=VERTEX_POINT('',#2814);
#773=EDGE_CURVE('',#638,#638,#520,.T.);
#774=EDGE_CURVE('',#638,#639,#334,.T.);
#775=EDGE_CURVE('',#639,#639,#521,.T.);
#776=EDGE_CURVE('',#640,#640,#522,.T.);
#777=EDGE_CURVE('',#640,#641,#335,.T.);
#778=EDGE_CURVE('',#641,#641,#523,.T.);
#779=EDGE_CURVE('',#642,#642,#524,.T.);
#780=EDGE_CURVE('',#642,#643,#336,.T.);
#781=EDGE_CURVE('',#643,#643,#525,.T.);
#782=EDGE_CURVE('',#644,#644,#526,.T.);
#783=EDGE_CURVE('',#644,#645,#337,.T.);
#784=EDGE_CURVE('',#645,#645,#527,.T.);
#785=EDGE_CURVE('',#646,#646,#528,.T.);
#786=EDGE_CURVE('',#646,#647,#338,.T.);
#787=EDGE_CURVE('',#647,#647,#529,.T.);
#788=EDGE_CURVE('',#648,#649,#339,.T.);
#789=EDGE_CURVE('',#649,#650,#340,.T.);
#790=EDGE_CURVE('',#650,#651,#341,.T.);
#791=EDGE_CURVE('',#651,#648,#342,.T.);
#792=EDGE_CURVE('',#652,#653,#343,.T.);
#793=EDGE_CURVE('',#653,#654,#344,.T.);
#794=EDGE_CURVE('',#654,#655,#345,.T.);
#795=EDGE_CURVE('',#655,#652,#346,.T.);
#796=EDGE_CURVE('',#656,#657,#347,.T.);
#797=EDGE_CURVE('',#657,#658,#348,.T.);
#798=EDGE_CURVE('',#658,#659,#349,.T.);
#799=EDGE_CURVE('',#659,#656,#350,.T.);
#800=EDGE_CURVE('',#660,#661,#351,.T.);
#801=EDGE_CURVE('',#661,#662,#352,.T.);
#802=EDGE_CURVE('',#662,#663,#353,.T.);
#803=EDGE_CURVE('',#663,#660,#354,.T.);
#804=EDGE_CURVE('',#664,#665,#355,.T.);
#805=EDGE_CURVE('',#665,#666,#530,.T.);
#806=EDGE_CURVE('',#666,#667,#356,.T.);
#807=EDGE_CURVE('',#667,#668,#531,.T.);
#808=EDGE_CURVE('',#668,#669,#357,.T.);
#809=EDGE_CURVE('',#669,#670,#532,.T.);
#810=EDGE_CURVE('',#670,#671,#358,.T.);
#811=EDGE_CURVE('',#671,#664,#533,.T.);
#812=EDGE_CURVE('',#672,#673,#359,.T.);
#813=EDGE_CURVE('',#673,#674,#534,.T.);
#814=EDGE_CURVE('',#674,#675,#360,.T.);
#815=EDGE_CURVE('',#675,#676,#535,.T.);
#816=EDGE_CURVE('',#676,#677,#361,.T.);
#817=EDGE_CURVE('',#677,#678,#536,.T.);
#818=EDGE_CURVE('',#678,#679,#362,.T.);
#819=EDGE_CURVE('',#679,#672,#537,.T.);
#820=EDGE_CURVE('',#654,#657,#538,.T.);
#821=EDGE_CURVE('',#656,#655,#539,.T.);
#822=EDGE_CURVE('',#650,#653,#540,.T.);
#823=EDGE_CURVE('',#652,#651,#541,.T.);
#824=EDGE_CURVE('',#660,#649,#542,.T.);
#825=EDGE_CURVE('',#648,#661,#543,.T.);
#826=EDGE_CURVE('',#658,#663,#544,.T.);
#827=EDGE_CURVE('',#662,#659,#545,.T.);
#828=EDGE_CURVE('',#653,#677,#546,.T.);
#829=EDGE_CURVE('',#678,#650,#547,.T.);
#830=EDGE_CURVE('',#679,#649,#548,.T.);
#831=EDGE_CURVE('',#654,#676,#549,.T.);
#832=EDGE_CURVE('',#672,#660,#550,.T.);
#833=EDGE_CURVE('',#657,#675,#551,.T.);
#834=EDGE_CURVE('',#673,#663,#552,.T.);
#835=EDGE_CURVE('',#658,#674,#553,.T.);
#836=EDGE_CURVE('',#661,#669,#554,.T.);
#837=EDGE_CURVE('',#670,#648,#555,.T.);
#838=EDGE_CURVE('',#671,#651,#556,.T.);
#839=EDGE_CURVE('',#662,#668,#557,.T.);
#840=EDGE_CURVE('',#664,#652,#558,.T.);
#841=EDGE_CURVE('',#659,#667,#559,.T.);
#842=EDGE_CURVE('',#665,#655,#560,.T.);
#843=EDGE_CURVE('',#656,#666,#561,.T.);
#844=EDGE_CURVE('',#680,#680,#562,.T.);
#845=EDGE_CURVE('',#680,#681,#363,.T.);
#846=EDGE_CURVE('',#681,#681,#563,.T.);
#847=EDGE_CURVE('',#682,#682,#564,.T.);
#848=EDGE_CURVE('',#682,#683,#565,.T.);
#849=EDGE_CURVE('',#684,#683,#566,.T.);
#850=EDGE_CURVE('',#683,#684,#567,.T.);
#851=EDGE_CURVE('',#685,#685,#568,.T.);
#852=EDGE_CURVE('',#685,#684,#364,.T.);
#853=EDGE_CURVE('',#686,#686,#569,.T.);
#854=EDGE_CURVE('',#686,#687,#365,.T.);
#855=EDGE_CURVE('',#687,#687,#570,.T.);
#856=EDGE_CURVE('',#688,#688,#571,.T.);
#857=EDGE_CURVE('',#688,#689,#366,.T.);
#858=EDGE_CURVE('',#689,#689,#572,.T.);
#859=EDGE_CURVE('',#690,#690,#573,.T.);
#860=EDGE_CURVE('',#690,#691,#367,.T.);
#861=EDGE_CURVE('',#691,#691,#574,.T.);
#862=EDGE_CURVE('',#692,#692,#575,.T.);
#863=EDGE_CURVE('',#692,#693,#368,.T.);
#864=EDGE_CURVE('',#693,#693,#576,.T.);
#865=EDGE_CURVE('',#694,#694,#577,.T.);
#866=EDGE_CURVE('',#694,#695,#369,.T.);
#867=EDGE_CURVE('',#695,#695,#578,.T.);
#868=EDGE_CURVE('',#696,#696,#579,.T.);
#869=EDGE_CURVE('',#696,#697,#370,.T.);
#870=EDGE_CURVE('',#697,#697,#580,.T.);
#871=EDGE_CURVE('',#698,#698,#581,.T.);
#872=EDGE_CURVE('',#698,#699,#582,.T.);
#873=EDGE_CURVE('',#699,#699,#583,.T.);
#874=EDGE_CURVE('',#700,#700,#584,.T.);
#875=EDGE_CURVE('',#700,#698,#371,.T.);
#876=EDGE_CURVE('',#701,#701,#585,.T.);
#877=EDGE_CURVE('',#701,#702,#586,.T.);
#878=EDGE_CURVE('',#703,#702,#587,.T.);
#879=EDGE_CURVE('',#702,#703,#588,.T.);
#880=EDGE_CURVE('',#704,#704,#589,.T.);
#881=EDGE_CURVE('',#704,#703,#372,.T.);
#882=EDGE_CURVE('',#705,#705,#590,.T.);
#883=EDGE_CURVE('',#705,#706,#373,.T.);
#884=EDGE_CURVE('',#706,#706,#591,.T.);
#885=EDGE_CURVE('',#707,#707,#592,.T.);
#886=EDGE_CURVE('',#707,#708,#374,.T.);
#887=EDGE_CURVE('',#708,#708,#593,.T.);
#888=EDGE_CURVE('',#709,#710,#594,.T.);
#889=EDGE_CURVE('',#709,#711,#375,.T.);
#890=EDGE_CURVE('',#711,#712,#595,.T.);
#891=EDGE_CURVE('',#710,#712,#376,.T.);
#892=EDGE_CURVE('',#713,#714,#596,.T.);
#893=EDGE_CURVE('',#713,#715,#377,.T.);
#894=EDGE_CURVE('',#715,#716,#597,.T.);
#895=EDGE_CURVE('',#714,#716,#378,.T.);
#896=EDGE_CURVE('',#717,#718,#598,.T.);
#897=EDGE_CURVE('',#717,#719,#379,.T.);
#898=EDGE_CURVE('',#719,#720,#599,.T.);
#899=EDGE_CURVE('',#718,#720,#380,.T.);
#900=EDGE_CURVE('',#721,#721,#600,.T.);
#901=EDGE_CURVE('',#721,#722,#381,.T.);
#902=EDGE_CURVE('',#722,#722,#601,.T.);
#903=EDGE_CURVE('',#723,#724,#602,.T.);
#904=EDGE_CURVE('',#724,#725,#382,.T.);
#905=EDGE_CURVE('',#725,#726,#603,.T.);
#906=EDGE_CURVE('',#726,#727,#604,.T.);
#907=EDGE_CURVE('',#727,#728,#605,.T.);
#908=EDGE_CURVE('',#728,#729,#383,.T.);
#909=EDGE_CURVE('',#729,#730,#606,.T.);
#910=EDGE_CURVE('',#730,#731,#384,.T.);
#911=EDGE_CURVE('',#731,#732,#607,.T.);
#912=EDGE_CURVE('',#732,#733,#608,.T.);
#913=EDGE_CURVE('',#733,#734,#609,.T.);
#914=EDGE_CURVE('',#734,#717,#385,.T.);
#915=EDGE_CURVE('',#718,#735,#386,.T.);
#916=EDGE_CURVE('',#735,#713,#610,.T.);
#917=EDGE_CURVE('',#714,#736,#611,.T.);
#918=EDGE_CURVE('',#736,#709,#387,.T.);
#919=EDGE_CURVE('',#710,#737,#388,.T.);
#920=EDGE_CURVE('',#737,#738,#612,.T.);
#921=EDGE_CURVE('',#738,#739,#613,.T.);
#922=EDGE_CURVE('',#739,#740,#614,.T.);
#923=EDGE_CURVE('',#740,#741,#389,.T.);
#924=EDGE_CURVE('',#741,#742,#615,.T.);
#925=EDGE_CURVE('',#742,#743,#390,.T.);
#926=EDGE_CURVE('',#743,#744,#616,.T.);
#927=EDGE_CURVE('',#744,#745,#617,.T.);
#928=EDGE_CURVE('',#745,#746,#618,.T.);
#929=EDGE_CURVE('',#746,#723,#391,.T.);
#930=EDGE_CURVE('',#747,#748,#619,.T.);
#931=EDGE_CURVE('',#749,#747,#392,.T.);
#932=EDGE_CURVE('',#750,#749,#620,.T.);
#933=EDGE_CURVE('',#751,#750,#621,.T.);
#934=EDGE_CURVE('',#752,#751,#622,.T.);
#935=EDGE_CURVE('',#753,#752,#393,.T.);
#936=EDGE_CURVE('',#754,#753,#623,.T.);
#937=EDGE_CURVE('',#755,#754,#394,.T.);
#938=EDGE_CURVE('',#756,#755,#624,.T.);
#939=EDGE_CURVE('',#757,#756,#625,.T.);
#940=EDGE_CURVE('',#758,#757,#626,.T.);
#941=EDGE_CURVE('',#712,#758,#395,.T.);
#942=EDGE_CURVE('',#759,#711,#396,.T.);
#943=EDGE_CURVE('',#716,#759,#627,.T.);
#944=EDGE_CURVE('',#760,#715,#628,.T.);
#945=EDGE_CURVE('',#720,#760,#397,.T.);
#946=EDGE_CURVE('',#761,#719,#398,.T.);
#947=EDGE_CURVE('',#762,#761,#629,.T.);
#948=EDGE_CURVE('',#763,#762,#630,.T.);
#949=EDGE_CURVE('',#764,#763,#631,.T.);
#950=EDGE_CURVE('',#765,#764,#399,.T.);
#951=EDGE_CURVE('',#766,#765,#632,.T.);
#952=EDGE_CURVE('',#767,#766,#400,.T.);
#953=EDGE_CURVE('',#768,#767,#633,.T.);
#954=EDGE_CURVE('',#769,#768,#634,.T.);
#955=EDGE_CURVE('',#770,#769,#635,.T.);
#956=EDGE_CURVE('',#748,#770,#401,.T.);
#957=EDGE_CURVE('',#724,#748,#402,.T.);
#958=EDGE_CURVE('',#723,#747,#403,.T.);
#959=EDGE_CURVE('',#725,#770,#404,.T.);
#960=EDGE_CURVE('',#726,#769,#405,.T.);
#961=EDGE_CURVE('',#727,#768,#406,.T.);
#962=EDGE_CURVE('',#728,#767,#407,.T.);
#963=EDGE_CURVE('',#729,#766,#408,.T.);
#964=EDGE_CURVE('',#730,#765,#409,.T.);
#965=EDGE_CURVE('',#731,#764,#410,.T.);
#966=EDGE_CURVE('',#732,#763,#411,.T.);
#967=EDGE_CURVE('',#733,#762,#412,.T.);
#968=EDGE_CURVE('',#734,#761,#413,.T.);
#969=EDGE_CURVE('',#735,#760,#414,.T.);
#970=EDGE_CURVE('',#736,#759,#415,.T.);
#971=EDGE_CURVE('',#737,#758,#416,.T.);
#972=EDGE_CURVE('',#738,#757,#417,.T.);
#973=EDGE_CURVE('',#739,#756,#418,.T.);
#974=EDGE_CURVE('',#740,#755,#419,.T.);
#975=EDGE_CURVE('',#741,#754,#420,.T.);
#976=EDGE_CURVE('',#742,#753,#421,.T.);
#977=EDGE_CURVE('',#743,#752,#422,.T.);
#978=EDGE_CURVE('',#744,#751,#423,.T.);
#979=EDGE_CURVE('',#745,#750,#424,.T.);
#980=EDGE_CURVE('',#746,#749,#425,.T.);
#981=EDGE_CURVE('',#771,#771,#636,.T.);
#982=EDGE_CURVE('',#771,#772,#426,.T.);
#983=EDGE_CURVE('',#772,#772,#637,.T.);
#984=ORIENTED_EDGE('',*,*,#773,.F.);
#985=ORIENTED_EDGE('',*,*,#774,.T.);
#986=ORIENTED_EDGE('',*,*,#775,.T.);
#987=ORIENTED_EDGE('',*,*,#774,.F.);
#988=ORIENTED_EDGE('',*,*,#776,.F.);
#989=ORIENTED_EDGE('',*,*,#777,.T.);
#990=ORIENTED_EDGE('',*,*,#778,.T.);
#991=ORIENTED_EDGE('',*,*,#777,.F.);
#992=ORIENTED_EDGE('',*,*,#779,.F.);
#993=ORIENTED_EDGE('',*,*,#780,.T.);
#994=ORIENTED_EDGE('',*,*,#781,.T.);
#995=ORIENTED_EDGE('',*,*,#780,.F.);
#996=ORIENTED_EDGE('',*,*,#782,.F.);
#997=ORIENTED_EDGE('',*,*,#783,.T.);
#998=ORIENTED_EDGE('',*,*,#784,.T.);
#999=ORIENTED_EDGE('',*,*,#783,.F.);
#1000=ORIENTED_EDGE('',*,*,#785,.F.);
#1001=ORIENTED_EDGE('',*,*,#786,.T.);
#1002=ORIENTED_EDGE('',*,*,#787,.T.);
#1003=ORIENTED_EDGE('',*,*,#786,.F.);
#1004=ORIENTED_EDGE('',*,*,#788,.T.);
#1005=ORIENTED_EDGE('',*,*,#789,.T.);
#1006=ORIENTED_EDGE('',*,*,#790,.T.);
#1007=ORIENTED_EDGE('',*,*,#791,.T.);
#1008=ORIENTED_EDGE('',*,*,#792,.T.);
#1009=ORIENTED_EDGE('',*,*,#793,.T.);
#1010=ORIENTED_EDGE('',*,*,#794,.T.);
#1011=ORIENTED_EDGE('',*,*,#795,.T.);
#1012=ORIENTED_EDGE('',*,*,#796,.T.);
#1013=ORIENTED_EDGE('',*,*,#797,.T.);
#1014=ORIENTED_EDGE('',*,*,#798,.T.);
#1015=ORIENTED_EDGE('',*,*,#799,.T.);
#1016=ORIENTED_EDGE('',*,*,#800,.T.);
#1017=ORIENTED_EDGE('',*,*,#801,.T.);
#1018=ORIENTED_EDGE('',*,*,#802,.T.);
#1019=ORIENTED_EDGE('',*,*,#803,.T.);
#1020=ORIENTED_EDGE('',*,*,#804,.T.);
#1021=ORIENTED_EDGE('',*,*,#805,.T.);
#1022=ORIENTED_EDGE('',*,*,#806,.T.);
#1023=ORIENTED_EDGE('',*,*,#807,.T.);
#1024=ORIENTED_EDGE('',*,*,#808,.T.);
#1025=ORIENTED_EDGE('',*,*,#809,.T.);
#1026=ORIENTED_EDGE('',*,*,#810,.T.);
#1027=ORIENTED_EDGE('',*,*,#811,.T.);
#1028=ORIENTED_EDGE('',*,*,#778,.F.);
#1029=ORIENTED_EDGE('',*,*,#781,.F.);
#1030=ORIENTED_EDGE('',*,*,#784,.F.);
#1031=ORIENTED_EDGE('',*,*,#787,.F.);
#1032=ORIENTED_EDGE('',*,*,#775,.F.);
#1033=ORIENTED_EDGE('',*,*,#812,.T.);
#1034=ORIENTED_EDGE('',*,*,#813,.T.);
#1035=ORIENTED_EDGE('',*,*,#814,.T.);
#1036=ORIENTED_EDGE('',*,*,#815,.T.);
#1037=ORIENTED_EDGE('',*,*,#816,.T.);
#1038=ORIENTED_EDGE('',*,*,#817,.T.);
#1039=ORIENTED_EDGE('',*,*,#818,.T.);
#1040=ORIENTED_EDGE('',*,*,#819,.T.);
#1041=ORIENTED_EDGE('',*,*,#776,.T.);
#1042=ORIENTED_EDGE('',*,*,#779,.T.);
#1043=ORIENTED_EDGE('',*,*,#782,.T.);
#1044=ORIENTED_EDGE('',*,*,#785,.T.);
#1045=ORIENTED_EDGE('',*,*,#794,.F.);
#1046=ORIENTED_EDGE('',*,*,#820,.T.);
#1047=ORIENTED_EDGE('',*,*,#796,.F.);
#1048=ORIENTED_EDGE('',*,*,#821,.T.);
#1049=ORIENTED_EDGE('',*,*,#790,.F.);
#1050=ORIENTED_EDGE('',*,*,#822,.T.);
#1051=ORIENTED_EDGE('',*,*,#792,.F.);
#1052=ORIENTED_EDGE('',*,*,#823,.T.);
#1053=ORIENTED_EDGE('',*,*,#800,.F.);
#1054=ORIENTED_EDGE('',*,*,#824,.T.);
#1055=ORIENTED_EDGE('',*,*,#788,.F.);
#1056=ORIENTED_EDGE('',*,*,#825,.T.);
#1057=ORIENTED_EDGE('',*,*,#798,.F.);
#1058=ORIENTED_EDGE('',*,*,#826,.T.);
#1059=ORIENTED_EDGE('',*,*,#802,.F.);
#1060=ORIENTED_EDGE('',*,*,#827,.T.);
#1061=ORIENTED_EDGE('',*,*,#828,.F.);
#1062=ORIENTED_EDGE('',*,*,#822,.F.);
#1063=ORIENTED_EDGE('',*,*,#829,.F.);
#1064=ORIENTED_EDGE('',*,*,#817,.F.);
#1065=ORIENTED_EDGE('',*,*,#829,.T.);
#1066=ORIENTED_EDGE('',*,*,#789,.F.);
#1067=ORIENTED_EDGE('',*,*,#830,.F.);
#1068=ORIENTED_EDGE('',*,*,#818,.F.);
#1069=ORIENTED_EDGE('',*,*,#828,.T.);
#1070=ORIENTED_EDGE('',*,*,#816,.F.);
#1071=ORIENTED_EDGE('',*,*,#831,.F.);
#1072=ORIENTED_EDGE('',*,*,#793,.F.);
#1073=ORIENTED_EDGE('',*,*,#830,.T.);
#1074=ORIENTED_EDGE('',*,*,#824,.F.);
#1075=ORIENTED_EDGE('',*,*,#832,.F.);
#1076=ORIENTED_EDGE('',*,*,#819,.F.);
#1077=ORIENTED_EDGE('',*,*,#831,.T.);
#1078=ORIENTED_EDGE('',*,*,#815,.F.);
#1079=ORIENTED_EDGE('',*,*,#833,.F.);
#1080=ORIENTED_EDGE('',*,*,#820,.F.);
#1081=ORIENTED_EDGE('',*,*,#832,.T.);
#1082=ORIENTED_EDGE('',*,*,#803,.F.);
#1083=ORIENTED_EDGE('',*,*,#834,.F.);
#1084=ORIENTED_EDGE('',*,*,#812,.F.);
#1085=ORIENTED_EDGE('',*,*,#833,.T.);
#1086=ORIENTED_EDGE('',*,*,#814,.F.);
#1087=ORIENTED_EDGE('',*,*,#835,.F.);
#1088=ORIENTED_EDGE('',*,*,#797,.F.);
#1089=ORIENTED_EDGE('',*,*,#834,.T.);
#1090=ORIENTED_EDGE('',*,*,#826,.F.);
#1091=ORIENTED_EDGE('',*,*,#835,.T.);
#1092=ORIENTED_EDGE('',*,*,#813,.F.);
#1093=ORIENTED_EDGE('',*,*,#836,.F.);
#1094=ORIENTED_EDGE('',*,*,#825,.F.);
#1095=ORIENTED_EDGE('',*,*,#837,.F.);
#1096=ORIENTED_EDGE('',*,*,#809,.F.);
#1097=ORIENTED_EDGE('',*,*,#837,.T.);
#1098=ORIENTED_EDGE('',*,*,#791,.F.);
#1099=ORIENTED_EDGE('',*,*,#838,.F.);
#1100=ORIENTED_EDGE('',*,*,#810,.F.);
#1101=ORIENTED_EDGE('',*,*,#836,.T.);
#1102=ORIENTED_EDGE('',*,*,#808,.F.);
#1103=ORIENTED_EDGE('',*,*,#839,.F.);
#1104=ORIENTED_EDGE('',*,*,#801,.F.);
#1105=ORIENTED_EDGE('',*,*,#838,.T.);
#1106=ORIENTED_EDGE('',*,*,#823,.F.);
#1107=ORIENTED_EDGE('',*,*,#840,.F.);
#1108=ORIENTED_EDGE('',*,*,#811,.F.);
#1109=ORIENTED_EDGE('',*,*,#839,.T.);
#1110=ORIENTED_EDGE('',*,*,#807,.F.);
#1111=ORIENTED_EDGE('',*,*,#841,.F.);
#1112=ORIENTED_EDGE('',*,*,#827,.F.);
#1113=ORIENTED_EDGE('',*,*,#840,.T.);
#1114=ORIENTED_EDGE('',*,*,#795,.F.);
#1115=ORIENTED_EDGE('',*,*,#842,.F.);
#1116=ORIENTED_EDGE('',*,*,#804,.F.);
#1117=ORIENTED_EDGE('',*,*,#841,.T.);
#1118=ORIENTED_EDGE('',*,*,#806,.F.);
#1119=ORIENTED_EDGE('',*,*,#843,.F.);
#1120=ORIENTED_EDGE('',*,*,#799,.F.);
#1121=ORIENTED_EDGE('',*,*,#842,.T.);
#1122=ORIENTED_EDGE('',*,*,#821,.F.);
#1123=ORIENTED_EDGE('',*,*,#843,.T.);
#1124=ORIENTED_EDGE('',*,*,#805,.F.);
#1125=ORIENTED_EDGE('',*,*,#773,.T.);
#1126=ORIENTED_EDGE('',*,*,#844,.F.);
#1127=ORIENTED_EDGE('',*,*,#845,.T.);
#1128=ORIENTED_EDGE('',*,*,#846,.T.);
#1129=ORIENTED_EDGE('',*,*,#845,.F.);
#1130=ORIENTED_EDGE('',*,*,#847,.F.);
#1131=ORIENTED_EDGE('',*,*,#848,.T.);
#1132=ORIENTED_EDGE('',*,*,#849,.F.);
#1133=ORIENTED_EDGE('',*,*,#850,.F.);
#1134=ORIENTED_EDGE('',*,*,#848,.F.);
#1135=ORIENTED_EDGE('',*,*,#851,.T.);
#1136=ORIENTED_EDGE('',*,*,#852,.T.);
#1137=ORIENTED_EDGE('',*,*,#849,.T.);
#1138=ORIENTED_EDGE('',*,*,#850,.T.);
#1139=ORIENTED_EDGE('',*,*,#852,.F.);
#1140=ORIENTED_EDGE('',*,*,#847,.T.);
#1141=ORIENTED_EDGE('',*,*,#846,.F.);
#1142=ORIENTED_EDGE('',*,*,#851,.F.);
#1143=ORIENTED_EDGE('',*,*,#844,.T.);
#1144=ORIENTED_EDGE('',*,*,#853,.F.);
#1145=ORIENTED_EDGE('',*,*,#854,.T.);
#1146=ORIENTED_EDGE('',*,*,#855,.T.);
#1147=ORIENTED_EDGE('',*,*,#854,.F.);
#1148=ORIENTED_EDGE('',*,*,#856,.F.);
#1149=ORIENTED_EDGE('',*,*,#857,.T.);
#1150=ORIENTED_EDGE('',*,*,#858,.T.);
#1151=ORIENTED_EDGE('',*,*,#857,.F.);
#1152=ORIENTED_EDGE('',*,*,#859,.F.);
#1153=ORIENTED_EDGE('',*,*,#860,.T.);
#1154=ORIENTED_EDGE('',*,*,#861,.T.);
#1155=ORIENTED_EDGE('',*,*,#860,.F.);
#1156=ORIENTED_EDGE('',*,*,#862,.F.);
#1157=ORIENTED_EDGE('',*,*,#863,.T.);
#1158=ORIENTED_EDGE('',*,*,#864,.T.);
#1159=ORIENTED_EDGE('',*,*,#863,.F.);
#1160=ORIENTED_EDGE('',*,*,#865,.F.);
#1161=ORIENTED_EDGE('',*,*,#866,.T.);
#1162=ORIENTED_EDGE('',*,*,#867,.T.);
#1163=ORIENTED_EDGE('',*,*,#866,.F.);
#1164=ORIENTED_EDGE('',*,*,#868,.F.);
#1165=ORIENTED_EDGE('',*,*,#869,.T.);
#1166=ORIENTED_EDGE('',*,*,#870,.T.);
#1167=ORIENTED_EDGE('',*,*,#869,.F.);
#1168=ORIENTED_EDGE('',*,*,#871,.F.);
#1169=ORIENTED_EDGE('',*,*,#872,.T.);
#1170=ORIENTED_EDGE('',*,*,#873,.F.);
#1171=ORIENTED_EDGE('',*,*,#872,.F.);
#1172=ORIENTED_EDGE('',*,*,#874,.F.);
#1173=ORIENTED_EDGE('',*,*,#875,.T.);
#1174=ORIENTED_EDGE('',*,*,#871,.T.);
#1175=ORIENTED_EDGE('',*,*,#875,.F.);
#1176=ORIENTED_EDGE('',*,*,#876,.F.);
#1177=ORIENTED_EDGE('',*,*,#877,.T.);
#1178=ORIENTED_EDGE('',*,*,#878,.F.);
#1179=ORIENTED_EDGE('',*,*,#879,.F.);
#1180=ORIENTED_EDGE('',*,*,#877,.F.);
#1181=ORIENTED_EDGE('',*,*,#880,.T.);
#1182=ORIENTED_EDGE('',*,*,#881,.T.);
#1183=ORIENTED_EDGE('',*,*,#878,.T.);
#1184=ORIENTED_EDGE('',*,*,#879,.T.);
#1185=ORIENTED_EDGE('',*,*,#881,.F.);
#1186=ORIENTED_EDGE('',*,*,#876,.T.);
#1187=ORIENTED_EDGE('',*,*,#855,.F.);
#1188=ORIENTED_EDGE('',*,*,#858,.F.);
#1189=ORIENTED_EDGE('',*,*,#861,.F.);
#1190=ORIENTED_EDGE('',*,*,#864,.F.);
#1191=ORIENTED_EDGE('',*,*,#867,.F.);
#1192=ORIENTED_EDGE('',*,*,#870,.F.);
#1193=ORIENTED_EDGE('',*,*,#873,.T.);
#1194=ORIENTED_EDGE('',*,*,#880,.F.);
#1195=ORIENTED_EDGE('',*,*,#853,.T.);
#1196=ORIENTED_EDGE('',*,*,#856,.T.);
#1197=ORIENTED_EDGE('',*,*,#859,.T.);
#1198=ORIENTED_EDGE('',*,*,#862,.T.);
#1199=ORIENTED_EDGE('',*,*,#865,.T.);
#1200=ORIENTED_EDGE('',*,*,#868,.T.);
#1201=ORIENTED_EDGE('',*,*,#874,.T.);
#1202=ORIENTED_EDGE('',*,*,#882,.T.);
#1203=ORIENTED_EDGE('',*,*,#883,.T.);
#1204=ORIENTED_EDGE('',*,*,#884,.F.);
#1205=ORIENTED_EDGE('',*,*,#883,.F.);
#1206=ORIENTED_EDGE('',*,*,#884,.T.);
#1207=ORIENTED_EDGE('',*,*,#882,.F.);
#1208=ORIENTED_EDGE('',*,*,#885,.F.);
#1209=ORIENTED_EDGE('',*,*,#886,.T.);
#1210=ORIENTED_EDGE('',*,*,#887,.T.);
#1211=ORIENTED_EDGE('',*,*,#886,.F.);
#1212=ORIENTED_EDGE('',*,*,#888,.F.);
#1213=ORIENTED_EDGE('',*,*,#889,.T.);
#1214=ORIENTED_EDGE('',*,*,#890,.T.);
#1215=ORIENTED_EDGE('',*,*,#891,.F.);
#1216=ORIENTED_EDGE('',*,*,#892,.F.);
#1217=ORIENTED_EDGE('',*,*,#893,.T.);
#1218=ORIENTED_EDGE('',*,*,#894,.T.);
#1219=ORIENTED_EDGE('',*,*,#895,.F.);
#1220=ORIENTED_EDGE('',*,*,#896,.F.);
#1221=ORIENTED_EDGE('',*,*,#897,.T.);
#1222=ORIENTED_EDGE('',*,*,#898,.T.);
#1223=ORIENTED_EDGE('',*,*,#899,.F.);
#1224=ORIENTED_EDGE('',*,*,#900,.F.);
#1225=ORIENTED_EDGE('',*,*,#901,.T.);
#1226=ORIENTED_EDGE('',*,*,#902,.T.);
#1227=ORIENTED_EDGE('',*,*,#901,.F.);
#1228=ORIENTED_EDGE('',*,*,#903,.T.);
#1229=ORIENTED_EDGE('',*,*,#904,.T.);
#1230=ORIENTED_EDGE('',*,*,#905,.T.);
#1231=ORIENTED_EDGE('',*,*,#906,.T.);
#1232=ORIENTED_EDGE('',*,*,#907,.T.);
#1233=ORIENTED_EDGE('',*,*,#908,.T.);
#1234=ORIENTED_EDGE('',*,*,#909,.T.);
#1235=ORIENTED_EDGE('',*,*,#910,.T.);
#1236=ORIENTED_EDGE('',*,*,#911,.T.);
#1237=ORIENTED_EDGE('',*,*,#912,.T.);
#1238=ORIENTED_EDGE('',*,*,#913,.T.);
#1239=ORIENTED_EDGE('',*,*,#914,.T.);
#1240=ORIENTED_EDGE('',*,*,#896,.T.);
#1241=ORIENTED_EDGE('',*,*,#915,.T.);
#1242=ORIENTED_EDGE('',*,*,#916,.T.);
#1243=ORIENTED_EDGE('',*,*,#892,.T.);
#1244=ORIENTED_EDGE('',*,*,#917,.T.);
#1245=ORIENTED_EDGE('',*,*,#918,.T.);
#1246=ORIENTED_EDGE('',*,*,#888,.T.);
#1247=ORIENTED_EDGE('',*,*,#919,.T.);
#1248=ORIENTED_EDGE('',*,*,#920,.T.);
#1249=ORIENTED_EDGE('',*,*,#921,.T.);
#1250=ORIENTED_EDGE('',*,*,#922,.T.);
#1251=ORIENTED_EDGE('',*,*,#923,.T.);
#1252=ORIENTED_EDGE('',*,*,#924,.T.);
#1253=ORIENTED_EDGE('',*,*,#925,.T.);
#1254=ORIENTED_EDGE('',*,*,#926,.T.);
#1255=ORIENTED_EDGE('',*,*,#927,.T.);
#1256=ORIENTED_EDGE('',*,*,#928,.T.);
#1257=ORIENTED_EDGE('',*,*,#929,.T.);
#1258=ORIENTED_EDGE('',*,*,#887,.F.);
#1259=ORIENTED_EDGE('',*,*,#930,.F.);
#1260=ORIENTED_EDGE('',*,*,#931,.F.);
#1261=ORIENTED_EDGE('',*,*,#932,.F.);
#1262=ORIENTED_EDGE('',*,*,#933,.F.);
#1263=ORIENTED_EDGE('',*,*,#934,.F.);
#1264=ORIENTED_EDGE('',*,*,#935,.F.);
#1265=ORIENTED_EDGE('',*,*,#936,.F.);
#1266=ORIENTED_EDGE('',*,*,#937,.F.);
#1267=ORIENTED_EDGE('',*,*,#938,.F.);
#1268=ORIENTED_EDGE('',*,*,#939,.F.);
#1269=ORIENTED_EDGE('',*,*,#940,.F.);
#1270=ORIENTED_EDGE('',*,*,#941,.F.);
#1271=ORIENTED_EDGE('',*,*,#890,.F.);
#1272=ORIENTED_EDGE('',*,*,#942,.F.);
#1273=ORIENTED_EDGE('',*,*,#943,.F.);
#1274=ORIENTED_EDGE('',*,*,#894,.F.);
#1275=ORIENTED_EDGE('',*,*,#944,.F.);
#1276=ORIENTED_EDGE('',*,*,#945,.F.);
#1277=ORIENTED_EDGE('',*,*,#898,.F.);
#1278=ORIENTED_EDGE('',*,*,#946,.F.);
#1279=ORIENTED_EDGE('',*,*,#947,.F.);
#1280=ORIENTED_EDGE('',*,*,#948,.F.);
#1281=ORIENTED_EDGE('',*,*,#949,.F.);
#1282=ORIENTED_EDGE('',*,*,#950,.F.);
#1283=ORIENTED_EDGE('',*,*,#951,.F.);
#1284=ORIENTED_EDGE('',*,*,#952,.F.);
#1285=ORIENTED_EDGE('',*,*,#953,.F.);
#1286=ORIENTED_EDGE('',*,*,#954,.F.);
#1287=ORIENTED_EDGE('',*,*,#955,.F.);
#1288=ORIENTED_EDGE('',*,*,#956,.F.);
#1289=ORIENTED_EDGE('',*,*,#902,.F.);
#1290=ORIENTED_EDGE('',*,*,#930,.T.);
#1291=ORIENTED_EDGE('',*,*,#957,.F.);
#1292=ORIENTED_EDGE('',*,*,#903,.F.);
#1293=ORIENTED_EDGE('',*,*,#958,.T.);
#1294=ORIENTED_EDGE('',*,*,#956,.T.);
#1295=ORIENTED_EDGE('',*,*,#959,.F.);
#1296=ORIENTED_EDGE('',*,*,#904,.F.);
#1297=ORIENTED_EDGE('',*,*,#957,.T.);
#1298=ORIENTED_EDGE('',*,*,#955,.T.);
#1299=ORIENTED_EDGE('',*,*,#960,.F.);
#1300=ORIENTED_EDGE('',*,*,#905,.F.);
#1301=ORIENTED_EDGE('',*,*,#959,.T.);
#1302=ORIENTED_EDGE('',*,*,#954,.T.);
#1303=ORIENTED_EDGE('',*,*,#961,.F.);
#1304=ORIENTED_EDGE('',*,*,#906,.F.);
#1305=ORIENTED_EDGE('',*,*,#960,.T.);
#1306=ORIENTED_EDGE('',*,*,#953,.T.);
#1307=ORIENTED_EDGE('',*,*,#962,.F.);
#1308=ORIENTED_EDGE('',*,*,#907,.F.);
#1309=ORIENTED_EDGE('',*,*,#961,.T.);
#1310=ORIENTED_EDGE('',*,*,#952,.T.);
#1311=ORIENTED_EDGE('',*,*,#963,.F.);
#1312=ORIENTED_EDGE('',*,*,#908,.F.);
#1313=ORIENTED_EDGE('',*,*,#962,.T.);
#1314=ORIENTED_EDGE('',*,*,#951,.T.);
#1315=ORIENTED_EDGE('',*,*,#964,.F.);
#1316=ORIENTED_EDGE('',*,*,#909,.F.);
#1317=ORIENTED_EDGE('',*,*,#963,.T.);
#1318=ORIENTED_EDGE('',*,*,#950,.T.);
#1319=ORIENTED_EDGE('',*,*,#965,.F.);
#1320=ORIENTED_EDGE('',*,*,#910,.F.);
#1321=ORIENTED_EDGE('',*,*,#964,.T.);
#1322=ORIENTED_EDGE('',*,*,#949,.T.);
#1323=ORIENTED_EDGE('',*,*,#966,.F.);
#1324=ORIENTED_EDGE('',*,*,#911,.F.);
#1325=ORIENTED_EDGE('',*,*,#965,.T.);
#1326=ORIENTED_EDGE('',*,*,#948,.T.);
#1327=ORIENTED_EDGE('',*,*,#967,.F.);
#1328=ORIENTED_EDGE('',*,*,#912,.F.);
#1329=ORIENTED_EDGE('',*,*,#966,.T.);
#1330=ORIENTED_EDGE('',*,*,#947,.T.);
#1331=ORIENTED_EDGE('',*,*,#968,.F.);
#1332=ORIENTED_EDGE('',*,*,#913,.F.);
#1333=ORIENTED_EDGE('',*,*,#967,.T.);
#1334=ORIENTED_EDGE('',*,*,#946,.T.);
#1335=ORIENTED_EDGE('',*,*,#897,.F.);
#1336=ORIENTED_EDGE('',*,*,#914,.F.);
#1337=ORIENTED_EDGE('',*,*,#968,.T.);
#1338=ORIENTED_EDGE('',*,*,#945,.T.);
#1339=ORIENTED_EDGE('',*,*,#969,.F.);
#1340=ORIENTED_EDGE('',*,*,#915,.F.);
#1341=ORIENTED_EDGE('',*,*,#899,.T.);
#1342=ORIENTED_EDGE('',*,*,#944,.T.);
#1343=ORIENTED_EDGE('',*,*,#893,.F.);
#1344=ORIENTED_EDGE('',*,*,#916,.F.);
#1345=ORIENTED_EDGE('',*,*,#969,.T.);
#1346=ORIENTED_EDGE('',*,*,#943,.T.);
#1347=ORIENTED_EDGE('',*,*,#970,.F.);
#1348=ORIENTED_EDGE('',*,*,#917,.F.);
#1349=ORIENTED_EDGE('',*,*,#895,.T.);
#1350=ORIENTED_EDGE('',*,*,#942,.T.);
#1351=ORIENTED_EDGE('',*,*,#889,.F.);
#1352=ORIENTED_EDGE('',*,*,#918,.F.);
#1353=ORIENTED_EDGE('',*,*,#970,.T.);
#1354=ORIENTED_EDGE('',*,*,#941,.T.);
#1355=ORIENTED_EDGE('',*,*,#971,.F.);
#1356=ORIENTED_EDGE('',*,*,#919,.F.);
#1357=ORIENTED_EDGE('',*,*,#891,.T.);
#1358=ORIENTED_EDGE('',*,*,#940,.T.);
#1359=ORIENTED_EDGE('',*,*,#972,.F.);
#1360=ORIENTED_EDGE('',*,*,#920,.F.);
#1361=ORIENTED_EDGE('',*,*,#971,.T.);
#1362=ORIENTED_EDGE('',*,*,#939,.T.);
#1363=ORIENTED_EDGE('',*,*,#973,.F.);
#1364=ORIENTED_EDGE('',*,*,#921,.F.);
#1365=ORIENTED_EDGE('',*,*,#972,.T.);
#1366=ORIENTED_EDGE('',*,*,#938,.T.);
#1367=ORIENTED_EDGE('',*,*,#974,.F.);
#1368=ORIENTED_EDGE('',*,*,#922,.F.);
#1369=ORIENTED_EDGE('',*,*,#973,.T.);
#1370=ORIENTED_EDGE('',*,*,#937,.T.);
#1371=ORIENTED_EDGE('',*,*,#975,.F.);
#1372=ORIENTED_EDGE('',*,*,#923,.F.);
#1373=ORIENTED_EDGE('',*,*,#974,.T.);
#1374=ORIENTED_EDGE('',*,*,#936,.T.);
#1375=ORIENTED_EDGE('',*,*,#976,.F.);
#1376=ORIENTED_EDGE('',*,*,#924,.F.);
#1377=ORIENTED_EDGE('',*,*,#975,.T.);
#1378=ORIENTED_EDGE('',*,*,#935,.T.);
#1379=ORIENTED_EDGE('',*,*,#977,.F.);
#1380=ORIENTED_EDGE('',*,*,#925,.F.);
#1381=ORIENTED_EDGE('',*,*,#976,.T.);
#1382=ORIENTED_EDGE('',*,*,#934,.T.);
#1383=ORIENTED_EDGE('',*,*,#978,.F.);
#1384=ORIENTED_EDGE('',*,*,#926,.F.);
#1385=ORIENTED_EDGE('',*,*,#977,.T.);
#1386=ORIENTED_EDGE('',*,*,#933,.T.);
#1387=ORIENTED_EDGE('',*,*,#979,.F.);
#1388=ORIENTED_EDGE('',*,*,#927,.F.);
#1389=ORIENTED_EDGE('',*,*,#978,.T.);
#1390=ORIENTED_EDGE('',*,*,#932,.T.);
#1391=ORIENTED_EDGE('',*,*,#980,.F.);
#1392=ORIENTED_EDGE('',*,*,#928,.F.);
#1393=ORIENTED_EDGE('',*,*,#979,.T.);
#1394=ORIENTED_EDGE('',*,*,#931,.T.);
#1395=ORIENTED_EDGE('',*,*,#958,.F.);
#1396=ORIENTED_EDGE('',*,*,#929,.F.);
#1397=ORIENTED_EDGE('',*,*,#980,.T.);
#1398=ORIENTED_EDGE('',*,*,#885,.T.);
#1399=ORIENTED_EDGE('',*,*,#900,.T.);
#1400=ORIENTED_EDGE('',*,*,#981,.T.);
#1401=ORIENTED_EDGE('',*,*,#982,.T.);
#1402=ORIENTED_EDGE('',*,*,#983,.F.);
#1403=ORIENTED_EDGE('',*,*,#982,.F.);
#1404=ORIENTED_EDGE('',*,*,#983,.T.);
#1405=ORIENTED_EDGE('',*,*,#981,.F.);
#1406=CYLINDRICAL_SURFACE('',#1622,12.5000000000002);
#1407=CYLINDRICAL_SURFACE('',#1625,8.00000000000001);
#1408=CYLINDRICAL_SURFACE('',#1628,8.00000000000001);
#1409=CYLINDRICAL_SURFACE('',#1631,8.00000000000001);
#1410=CYLINDRICAL_SURFACE('',#1634,8.00000000000001);
#1411=CYLINDRICAL_SURFACE('',#1651,20.);
#1412=CYLINDRICAL_SURFACE('',#1654,20.);
#1413=CYLINDRICAL_SURFACE('',#1657,20.);
#1414=CYLINDRICAL_SURFACE('',#1660,20.);
#1415=CYLINDRICAL_SURFACE('',#1666,1.50000000000006);
#1416=CYLINDRICAL_SURFACE('',#1668,1.5);
#1417=CYLINDRICAL_SURFACE('',#1674,1.5);
#1418=CYLINDRICAL_SURFACE('',#1676,1.50000000000006);
#1419=CYLINDRICAL_SURFACE('',#1682,1.50000000000006);
#1420=CYLINDRICAL_SURFACE('',#1684,1.5);
#1421=CYLINDRICAL_SURFACE('',#1690,1.5);
#1422=CYLINDRICAL_SURFACE('',#1692,1.50000000000006);
#1423=CYLINDRICAL_SURFACE('',#1697,12.5);
#1424=CYLINDRICAL_SURFACE('',#1705,107.5);
#1425=CYLINDRICAL_SURFACE('',#1710,4.92500000000001);
#1426=CYLINDRICAL_SURFACE('',#1713,4.92500000000001);
#1427=CYLINDRICAL_SURFACE('',#1716,3.5);
#1428=CYLINDRICAL_SURFACE('',#1719,3.5);
#1429=CYLINDRICAL_SURFACE('',#1722,3.5);
#1430=CYLINDRICAL_SURFACE('',#1725,3.5);
#1431=CYLINDRICAL_SURFACE('',#1732,12.5);
#1432=CYLINDRICAL_SURFACE('',#1739,95.0000000000003);
#1433=CYLINDRICAL_SURFACE('',#1744,4.83000000000002);
#1434=CYLINDRICAL_SURFACE('',#1750,12.7);
#1435=CYLINDRICAL_SURFACE('',#1753,4.826);
#1436=CYLINDRICAL_SURFACE('',#1756,76.1999999999999);
#1437=CYLINDRICAL_SURFACE('',#1759,4.826);
#1438=CYLINDRICAL_SURFACE('',#1762,8.88999999999999);
#1439=CYLINDRICAL_SURFACE('',#1801,4.826);
#1440=CYLINDRICAL_SURFACE('',#1803,27.0465001077289);
#1441=CYLINDRICAL_SURFACE('',#1804,76.2);
#1442=CYLINDRICAL_SURFACE('',#1805,27.0465001077289);
#1443=CYLINDRICAL_SURFACE('',#1807,4.826);
#1444=CYLINDRICAL_SURFACE('',#1809,27.0465001077289);
#1445=CYLINDRICAL_SURFACE('',#1810,76.1999999999999);
#1446=CYLINDRICAL_SURFACE('',#1811,27.0465001077289);
#1447=CYLINDRICAL_SURFACE('',#1814,27.0465001077289);
#1448=CYLINDRICAL_SURFACE('',#1815,27.0465001077289);
#1449=CYLINDRICAL_SURFACE('',#1818,27.0465001077289);
#1450=CYLINDRICAL_SURFACE('',#1819,76.1999999999999);
#1451=CYLINDRICAL_SURFACE('',#1820,27.0465001077289);
#1452=CYLINDRICAL_SURFACE('',#1822,4.826);
#1453=CYLINDRICAL_SURFACE('',#1824,27.0465001077289);
#1454=CYLINDRICAL_SURFACE('',#1825,76.1999999999999);
#1455=CYLINDRICAL_SURFACE('',#1826,27.0465001077289);
#1456=CYLINDRICAL_SURFACE('',#1830,8.89);
#1457=ADVANCED_FACE('',(#126),#1406,.F.);
#1458=ADVANCED_FACE('',(#127),#1407,.F.);
#1459=ADVANCED_FACE('',(#128),#1408,.F.);
#1460=ADVANCED_FACE('',(#129),#1409,.F.);
#1461=ADVANCED_FACE('',(#130),#1410,.F.);
#1462=ADVANCED_FACE('',(#131),#98,.T.);
#1463=ADVANCED_FACE('',(#132),#99,.T.);
#1464=ADVANCED_FACE('',(#133),#100,.F.);
#1465=ADVANCED_FACE('',(#134),#101,.F.);
#1466=ADVANCED_FACE('',(#135,#70,#71,#72,#73,#74),#102,.T.);
#1467=ADVANCED_FACE('',(#136,#75,#76,#77,#78),#103,.F.);
#1468=ADVANCED_FACE('',(#137),#1411,.T.);
#1469=ADVANCED_FACE('',(#138),#1412,.T.);
#1470=ADVANCED_FACE('',(#139),#1413,.T.);
#1471=ADVANCED_FACE('',(#140),#1414,.T.);
#1472=ADVANCED_FACE('',(#141),#59,.T.);
#1473=ADVANCED_FACE('',(#142),#1415,.T.);
#1474=ADVANCED_FACE('',(#143),#1416,.T.);
#1475=ADVANCED_FACE('',(#144),#60,.T.);
#1476=ADVANCED_FACE('',(#145),#61,.T.);
#1477=ADVANCED_FACE('',(#146),#1417,.T.);
#1478=ADVANCED_FACE('',(#147),#1418,.T.);
#1479=ADVANCED_FACE('',(#148),#62,.T.);
#1480=ADVANCED_FACE('',(#149),#63,.T.);
#1481=ADVANCED_FACE('',(#150),#1419,.T.);
#1482=ADVANCED_FACE('',(#151),#1420,.T.);
#1483=ADVANCED_FACE('',(#152),#64,.T.);
#1484=ADVANCED_FACE('',(#153),#65,.T.);
#1485=ADVANCED_FACE('',(#154),#1421,.T.);
#1486=ADVANCED_FACE('',(#155),#1422,.T.);
#1487=ADVANCED_FACE('',(#156),#66,.T.);
#1488=ADVANCED_FACE('',(#157),#104,.T.);
#1489=ADVANCED_FACE('',(#158),#1423,.F.);
#1490=ADVANCED_FACE('',(#159),#67,.T.);
#1491=ADVANCED_FACE('',(#160),#1424,.T.);
#1492=ADVANCED_FACE('',(#161,#79),#105,.T.);
#1493=ADVANCED_FACE('',(#162,#80),#106,.F.);
#1494=ADVANCED_FACE('',(#163),#1425,.F.);
#1495=ADVANCED_FACE('',(#164),#1426,.F.);
#1496=ADVANCED_FACE('',(#165),#1427,.F.);
#1497=ADVANCED_FACE('',(#166),#1428,.F.);
#1498=ADVANCED_FACE('',(#167),#1429,.F.);
#1499=ADVANCED_FACE('',(#168),#1430,.F.);
#1500=ADVANCED_FACE('',(#169),#68,.T.);
#1501=ADVANCED_FACE('',(#170),#1431,.F.);
#1502=ADVANCED_FACE('',(#171),#69,.T.);
#1503=ADVANCED_FACE('',(#172),#1432,.T.);
#1504=ADVANCED_FACE('',(#173,#81,#82,#83,#84,#85,#86,#87),#107,.T.);
#1505=ADVANCED_FACE('',(#174,#88,#89,#90,#91,#92,#93,#94),#108,.F.);
#1506=ADVANCED_FACE('',(#175),#1433,.T.);
#1507=ADVANCED_FACE('',(#176),#109,.T.);
#1508=ADVANCED_FACE('',(#177),#110,.F.);
#1509=ADVANCED_FACE('',(#178),#1434,.F.);
#1510=ADVANCED_FACE('',(#179),#1435,.F.);
#1511=ADVANCED_FACE('',(#180),#1436,.F.);
#1512=ADVANCED_FACE('',(#181),#1437,.F.);
#1513=ADVANCED_FACE('',(#182),#1438,.F.);
#1514=ADVANCED_FACE('',(#183,#95),#111,.T.);
#1515=ADVANCED_FACE('',(#184,#96),#112,.F.);
#1516=ADVANCED_FACE('',(#185),#1439,.F.);
#1517=ADVANCED_FACE('',(#186),#113,.F.);
#1518=ADVANCED_FACE('',(#187),#1440,.T.);
#1519=ADVANCED_FACE('',(#188),#1441,.F.);
#1520=ADVANCED_FACE('',(#189),#1442,.T.);
#1521=ADVANCED_FACE('',(#190),#114,.F.);
#1522=ADVANCED_FACE('',(#191),#1443,.F.);
#1523=ADVANCED_FACE('',(#192),#115,.F.);
#1524=ADVANCED_FACE('',(#193),#1444,.T.);
#1525=ADVANCED_FACE('',(#194),#1445,.F.);
#1526=ADVANCED_FACE('',(#195),#1446,.T.);
#1527=ADVANCED_FACE('',(#196),#116,.F.);
#1528=ADVANCED_FACE('',(#197),#117,.F.);
#1529=ADVANCED_FACE('',(#198),#1447,.T.);
#1530=ADVANCED_FACE('',(#199),#1448,.T.);
#1531=ADVANCED_FACE('',(#200),#118,.F.);
#1532=ADVANCED_FACE('',(#201),#119,.F.);
#1533=ADVANCED_FACE('',(#202),#1449,.T.);
#1534=ADVANCED_FACE('',(#203),#1450,.F.);
#1535=ADVANCED_FACE('',(#204),#1451,.T.);
#1536=ADVANCED_FACE('',(#205),#120,.F.);
#1537=ADVANCED_FACE('',(#206),#1452,.F.);
#1538=ADVANCED_FACE('',(#207),#121,.F.);
#1539=ADVANCED_FACE('',(#208),#1453,.T.);
#1540=ADVANCED_FACE('',(#209),#1454,.F.);
#1541=ADVANCED_FACE('',(#210),#1455,.T.);
#1542=ADVANCED_FACE('',(#211),#122,.F.);
#1543=ADVANCED_FACE('',(#212,#97),#123,.T.);
#1544=ADVANCED_FACE('',(#213),#1456,.T.);
#1545=ADVANCED_FACE('',(#214),#124,.T.);
#1546=ADVANCED_FACE('',(#215),#125,.F.);
#1547=CLOSED_SHELL('',(#1457,#1458,#1459,#1460,#1461,#1462,#1463,#1464,
#1465,#1466,#1467,#1468,#1469,#1470,#1471,#1472,#1473,#1474,#1475,#1476,
#1477,#1478,#1479,#1480,#1481,#1482,#1483,#1484,#1485,#1486,#1487,#1488));
#1548=CLOSED_SHELL('',(#1489,#1490,#1491,#1492,#1493));
#1549=CLOSED_SHELL('',(#1494,#1495,#1496,#1497,#1498,#1499,#1500,#1501,
#1502,#1503,#1504,#1505));
#1550=CLOSED_SHELL('',(#1506,#1507,#1508));
#1551=CLOSED_SHELL('',(#1509,#1510,#1511,#1512,#1513,#1514,#1515,#1516,
#1517,#1518,#1519,#1520,#1521,#1522,#1523,#1524,#1525,#1526,#1527,#1528,
#1529,#1530,#1531,#1532,#1533,#1534,#1535,#1536,#1537,#1538,#1539,#1540,
#1541,#1542,#1543));
#1552=CLOSED_SHELL('',(#1544,#1545,#1546));
#1553=DERIVED_UNIT_ELEMENT(#1565,1.);
#1554=DERIVED_UNIT_ELEMENT(#2842,-3.);
#1555=DERIVED_UNIT_ELEMENT(#1565,1.);
#1556=DERIVED_UNIT_ELEMENT(#2842,-3.);
#1557=DERIVED_UNIT_ELEMENT(#1565,1.);
#1558=DERIVED_UNIT_ELEMENT(#2842,-3.);
#1559=DERIVED_UNIT_ELEMENT(#1565,1.);
#1560=DERIVED_UNIT_ELEMENT(#2842,-3.);
#1561=DERIVED_UNIT_ELEMENT(#1565,1.);
#1562=DERIVED_UNIT_ELEMENT(#2842,-3.);
#1563=DERIVED_UNIT_ELEMENT(#1565,1.);
#1564=DERIVED_UNIT_ELEMENT(#2842,-3.);
#1565=(
MASS_UNIT()
NAMED_UNIT(*)
SI_UNIT(.KILO.,.GRAM.)
);
#1566=DERIVED_UNIT((#1553,#1554));
#1567=DERIVED_UNIT((#1555,#1556));
#1568=DERIVED_UNIT((#1557,#1558));
#1569=DERIVED_UNIT((#1559,#1560));
#1570=DERIVED_UNIT((#1561,#1562));
#1571=DERIVED_UNIT((#1563,#1564));
#1572=MEASURE_REPRESENTATION_ITEM('density measure',
POSITIVE_RATIO_MEASURE(7850.),#1566);
#1573=MEASURE_REPRESENTATION_ITEM('density measure',
POSITIVE_RATIO_MEASURE(7850.),#1567);
#1574=MEASURE_REPRESENTATION_ITEM('density measure',
POSITIVE_RATIO_MEASURE(7850.),#1568);
#1575=MEASURE_REPRESENTATION_ITEM('density measure',
POSITIVE_RATIO_MEASURE(7850.),#1569);
#1576=MEASURE_REPRESENTATION_ITEM('density measure',
POSITIVE_RATIO_MEASURE(7850.),#1570);
#1577=MEASURE_REPRESENTATION_ITEM('density measure',
POSITIVE_RATIO_MEASURE(7850.),#1571);
#1578=PROPERTY_DEFINITION_REPRESENTATION(#1608,#1590);
#1579=PROPERTY_DEFINITION_REPRESENTATION(#1609,#1591);
#1580=PROPERTY_DEFINITION_REPRESENTATION(#1610,#1592);
#1581=PROPERTY_DEFINITION_REPRESENTATION(#1611,#1593);
#1582=PROPERTY_DEFINITION_REPRESENTATION(#1612,#1594);
#1583=PROPERTY_DEFINITION_REPRESENTATION(#1613,#1595);
#1584=PROPERTY_DEFINITION_REPRESENTATION(#1614,#1596);
#1585=PROPERTY_DEFINITION_REPRESENTATION(#1615,#1597);
#1586=PROPERTY_DEFINITION_REPRESENTATION(#1616,#1598);
#1587=PROPERTY_DEFINITION_REPRESENTATION(#1617,#1599);
#1588=PROPERTY_DEFINITION_REPRESENTATION(#1618,#1600);
#1589=PROPERTY_DEFINITION_REPRESENTATION(#1619,#1601);
#1590=REPRESENTATION('material name',(#1602),#2834);
#1591=REPRESENTATION('density',(#1572),#2834);
#1592=REPRESENTATION('material name',(#1603),#2835);
#1593=REPRESENTATION('density',(#1573),#2835);
#1594=REPRESENTATION('material name',(#1604),#2836);
#1595=REPRESENTATION('density',(#1574),#2836);
#1596=REPRESENTATION('material name',(#1605),#2837);
#1597=REPRESENTATION('density',(#1575),#2837);
#1598=REPRESENTATION('material name',(#1606),#2838);
#1599=REPRESENTATION('density',(#1576),#2838);
#1600=REPRESENTATION('material name',(#1607),#2839);
#1601=REPRESENTATION('density',(#1577),#2839);
#1602=DESCRIPTIVE_REPRESENTATION_ITEM('Steel','Steel');
#1603=DESCRIPTIVE_REPRESENTATION_ITEM('Steel','Steel');
#1604=DESCRIPTIVE_REPRESENTATION_ITEM('Steel','Steel');
#1605=DESCRIPTIVE_REPRESENTATION_ITEM('Steel','Steel');
#1606=DESCRIPTIVE_REPRESENTATION_ITEM('Steel','Steel');
#1607=DESCRIPTIVE_REPRESENTATION_ITEM('Steel','Steel');
#1608=PROPERTY_DEFINITION('material property','material name',#2874);
#1609=PROPERTY_DEFINITION('material property','density of part',#2874);
#1610=PROPERTY_DEFINITION('material property','material name',#2875);
#1611=PROPERTY_DEFINITION('material property','density of part',#2875);
#1612=PROPERTY_DEFINITION('material property','material name',#2876);
#1613=PROPERTY_DEFINITION('material property','density of part',#2876);
#1614=PROPERTY_DEFINITION('material property','material name',#2877);
#1615=PROPERTY_DEFINITION('material property','density of part',#2877);
#1616=PROPERTY_DEFINITION('material property','material name',#2878);
#1617=PROPERTY_DEFINITION('material property','density of part',#2878);
#1618=PROPERTY_DEFINITION('material property','material name',#2879);
#1619=PROPERTY_DEFINITION('material property','density of part',#2879);
#1620=AXIS2_PLACEMENT_3D('',#2376,#1841,#1842);
#1621=AXIS2_PLACEMENT_3D('',#2377,#1843,#1844);
#1622=AXIS2_PLACEMENT_3D('',#2378,#1845,#1846);
#1623=AXIS2_PLACEMENT_3D('',#2380,#1847,#1848);
#1624=AXIS2_PLACEMENT_3D('',#2383,#1850,#1851);
#1625=AXIS2_PLACEMENT_3D('',#2384,#1852,#1853);
#1626=AXIS2_PLACEMENT_3D('',#2386,#1854,#1855);
#1627=AXIS2_PLACEMENT_3D('',#2389,#1857,#1858);
#1628=AXIS2_PLACEMENT_3D('',#2390,#1859,#1860);
#1629=AXIS2_PLACEMENT_3D('',#2392,#1861,#1862);
#1630=AXIS2_PLACEMENT_3D('',#2395,#1864,#1865);
#1631=AXIS2_PLACEMENT_3D('',#2396,#1866,#1867);
#1632=AXIS2_PLACEMENT_3D('',#2398,#1868,#1869);
#1633=AXIS2_PLACEMENT_3D('',#2401,#1871,#1872);
#1634=AXIS2_PLACEMENT_3D('',#2402,#1873,#1874);
#1635=AXIS2_PLACEMENT_3D('',#2404,#1875,#1876);
#1636=AXIS2_PLACEMENT_3D('',#2407,#1878,#1879);
#1637=AXIS2_PLACEMENT_3D('',#2408,#1880,#1881);
#1638=AXIS2_PLACEMENT_3D('',#2417,#1886,#1887);
#1639=AXIS2_PLACEMENT_3D('',#2426,#1892,#1893);
#1640=AXIS2_PLACEMENT_3D('',#2435,#1898,#1899);
#1641=AXIS2_PLACEMENT_3D('',#2444,#1904,#1905);
#1642=AXIS2_PLACEMENT_3D('',#2449,#1907,#1908);
#1643=AXIS2_PLACEMENT_3D('',#2453,#1910,#1911);
#1644=AXIS2_PLACEMENT_3D('',#2457,#1913,#1914);
#1645=AXIS2_PLACEMENT_3D('',#2460,#1916,#1917);
#1646=AXIS2_PLACEMENT_3D('',#2461,#1918,#1919);
#1647=AXIS2_PLACEMENT_3D('',#2466,#1921,#1922);
#1648=AXIS2_PLACEMENT_3D('',#2470,#1924,#1925);
#1649=AXIS2_PLACEMENT_3D('',#2474,#1927,#1928);
#1650=AXIS2_PLACEMENT_3D('',#2477,#1930,#1931);
#1651=AXIS2_PLACEMENT_3D('',#2478,#1932,#1933);
#1652=AXIS2_PLACEMENT_3D('',#2479,#1934,#1935);
#1653=AXIS2_PLACEMENT_3D('',#2480,#1936,#1937);
#1654=AXIS2_PLACEMENT_3D('',#2481,#1938,#1939);
#1655=AXIS2_PLACEMENT_3D('',#2482,#1940,#1941);
#1656=AXIS2_PLACEMENT_3D('',#2483,#1942,#1943);
#1657=AXIS2_PLACEMENT_3D('',#2484,#1944,#1945);
#1658=AXIS2_PLACEMENT_3D('',#2485,#1946,#1947);
#1659=AXIS2_PLACEMENT_3D('',#2486,#1948,#1949);
#1660=AXIS2_PLACEMENT_3D('',#2487,#1950,#1951);
#1661=AXIS2_PLACEMENT_3D('',#2488,#1952,#1953);
#1662=AXIS2_PLACEMENT_3D('',#2489,#1954,#1955);
#1663=AXIS2_PLACEMENT_3D('',#2490,#1956,#1957);
#1664=AXIS2_PLACEMENT_3D('',#2491,#1958,#1959);
#1665=AXIS2_PLACEMENT_3D('',#2492,#1960,#1961);
#1666=AXIS2_PLACEMENT_3D('',#2493,#1962,#1963);
#1667=AXIS2_PLACEMENT_3D('',#2494,#1964,#1965);
#1668=AXIS2_PLACEMENT_3D('',#2495,#1966,#1967);
#1669=AXIS2_PLACEMENT_3D('',#2496,#1968,#1969);
#1670=AXIS2_PLACEMENT_3D('',#2497,#1970,#1971);
#1671=AXIS2_PLACEMENT_3D('',#2498,#1972,#1973);
#1672=AXIS2_PLACEMENT_3D('',#2499,#1974,#1975);
#1673=AXIS2_PLACEMENT_3D('',#2500,#1976,#1977);
#1674=AXIS2_PLACEMENT_3D('',#2501,#1978,#1979);
#1675=AXIS2_PLACEMENT_3D('',#2502,#1980,#1981);
#1676=AXIS2_PLACEMENT_3D('',#2503,#1982,#1983);
#1677=AXIS2_PLACEMENT_3D('',#2504,#1984,#1985);
#1678=AXIS2_PLACEMENT_3D('',#2505,#1986,#1987);
#1679=AXIS2_PLACEMENT_3D('',#2506,#1988,#1989);
#1680=AXIS2_PLACEMENT_3D('',#2507,#1990,#1991);
#1681=AXIS2_PLACEMENT_3D('',#2508,#1992,#1993);
#1682=AXIS2_PLACEMENT_3D('',#2509,#1994,#1995);
#1683=AXIS2_PLACEMENT_3D('',#2510,#1996,#1997);
#1684=AXIS2_PLACEMENT_3D('',#2511,#1998,#1999);
#1685=AXIS2_PLACEMENT_3D('',#2512,#2000,#2001);
#1686=AXIS2_PLACEMENT_3D('',#2513,#2002,#2003);
#1687=AXIS2_PLACEMENT_3D('',#2514,#2004,#2005);
#1688=AXIS2_PLACEMENT_3D('',#2515,#2006,#2007);
#1689=AXIS2_PLACEMENT_3D('',#2516,#2008,#2009);
#1690=AXIS2_PLACEMENT_3D('',#2517,#2010,#2011);
#1691=AXIS2_PLACEMENT_3D('',#2518,#2012,#2013);
#1692=AXIS2_PLACEMENT_3D('',#2519,#2014,#2015);
#1693=AXIS2_PLACEMENT_3D('',#2520,#2016,#2017);
#1694=AXIS2_PLACEMENT_3D('',#2521,#2018,#2019);
#1695=AXIS2_PLACEMENT_3D('',#2522,#2020,#2021);
#1696=AXIS2_PLACEMENT_3D('',#2523,#2022,#2023);
#1697=AXIS2_PLACEMENT_3D('',#2524,#2024,#2025);
#1698=AXIS2_PLACEMENT_3D('',#2526,#2026,#2027);
#1699=AXIS2_PLACEMENT_3D('',#2529,#2029,#2030);
#1700=AXIS2_PLACEMENT_3D('',#2530,#2031,#2032);
#1701=AXIS2_PLACEMENT_3D('',#2532,#2033,#2034);
#1702=AXIS2_PLACEMENT_3D('',#2534,#2035,#2036);
#1703=AXIS2_PLACEMENT_3D('',#2536,#2037,#2038);
#1704=AXIS2_PLACEMENT_3D('',#2537,#2039,#2040);
#1705=AXIS2_PLACEMENT_3D('',#2538,#2041,#2042);
#1706=AXIS2_PLACEMENT_3D('',#2540,#2043,#2044);
#1707=AXIS2_PLACEMENT_3D('',#2542,#2046,#2047);
#1708=AXIS2_PLACEMENT_3D('',#2543,#2048,#2049);
#1709=AXIS2_PLACEMENT_3D('',#2544,#2050,#2051);
#1710=AXIS2_PLACEMENT_3D('',#2545,#2052,#2053);
#1711=AXIS2_PLACEMENT_3D('',#2547,#2054,#2055);
#1712=AXIS2_PLACEMENT_3D('',#2550,#2057,#2058);
#1713=AXIS2_PLACEMENT_3D('',#2551,#2059,#2060);
#1714=AXIS2_PLACEMENT_3D('',#2553,#2061,#2062);
#1715=AXIS2_PLACEMENT_3D('',#2556,#2064,#2065);
#1716=AXIS2_PLACEMENT_3D('',#2557,#2066,#2067);
#1717=AXIS2_PLACEMENT_3D('',#2559,#2068,#2069);
#1718=AXIS2_PLACEMENT_3D('',#2562,#2071,#2072);
#1719=AXIS2_PLACEMENT_3D('',#2563,#2073,#2074);
#1720=AXIS2_PLACEMENT_3D('',#2565,#2075,#2076);
#1721=AXIS2_PLACEMENT_3D('',#2568,#2078,#2079);
#1722=AXIS2_PLACEMENT_3D('',#2569,#2080,#2081);
#1723=AXIS2_PLACEMENT_3D('',#2571,#2082,#2083);
#1724=AXIS2_PLACEMENT_3D('',#2574,#2085,#2086);
#1725=AXIS2_PLACEMENT_3D('',#2575,#2087,#2088);
#1726=AXIS2_PLACEMENT_3D('',#2577,#2089,#2090);
#1727=AXIS2_PLACEMENT_3D('',#2580,#2092,#2093);
#1728=AXIS2_PLACEMENT_3D('',#2581,#2094,#2095);
#1729=AXIS2_PLACEMENT_3D('',#2583,#2096,#2097);
#1730=AXIS2_PLACEMENT_3D('',#2585,#2098,#2099);
#1731=AXIS2_PLACEMENT_3D('',#2586,#2100,#2101);
#1732=AXIS2_PLACEMENT_3D('',#2587,#2102,#2103);
#1733=AXIS2_PLACEMENT_3D('',#2589,#2104,#2105);
#1734=AXIS2_PLACEMENT_3D('',#2591,#2107,#2108);
#1735=AXIS2_PLACEMENT_3D('',#2593,#2109,#2110);
#1736=AXIS2_PLACEMENT_3D('',#2595,#2111,#2112);
#1737=AXIS2_PLACEMENT_3D('',#2597,#2113,#2114);
#1738=AXIS2_PLACEMENT_3D('',#2598,#2115,#2116);
#1739=AXIS2_PLACEMENT_3D('',#2599,#2117,#2118);
#1740=AXIS2_PLACEMENT_3D('',#2601,#2119,#2120);
#1741=AXIS2_PLACEMENT_3D('',#2603,#2122,#2123);
#1742=AXIS2_PLACEMENT_3D('',#2604,#2124,#2125);
#1743=AXIS2_PLACEMENT_3D('',#2605,#2126,#2127);
#1744=AXIS2_PLACEMENT_3D('',#2606,#2128,#2129);
#1745=AXIS2_PLACEMENT_3D('',#2608,#2130,#2131);
#1746=AXIS2_PLACEMENT_3D('',#2611,#2133,#2134);
#1747=AXIS2_PLACEMENT_3D('',#2612,#2135,#2136);
#1748=AXIS2_PLACEMENT_3D('',#2613,#2137,#2138);
#1749=AXIS2_PLACEMENT_3D('',#2614,#2139,#2140);
#1750=AXIS2_PLACEMENT_3D('',#2615,#2141,#2142);
#1751=AXIS2_PLACEMENT_3D('',#2617,#2143,#2144);
#1752=AXIS2_PLACEMENT_3D('',#2620,#2146,#2147);
#1753=AXIS2_PLACEMENT_3D('',#2621,#2148,#2149);
#1754=AXIS2_PLACEMENT_3D('',#2624,#2150,#2151);
#1755=AXIS2_PLACEMENT_3D('',#2628,#2153,#2154);
#1756=AXIS2_PLACEMENT_3D('',#2630,#2156,#2157);
#1757=AXIS2_PLACEMENT_3D('',#2633,#2158,#2159);
#1758=AXIS2_PLACEMENT_3D('',#2637,#2161,#2162);
#1759=AXIS2_PLACEMENT_3D('',#2639,#2164,#2165);
#1760=AXIS2_PLACEMENT_3D('',#2642,#2166,#2167);
#1761=AXIS2_PLACEMENT_3D('',#2646,#2169,#2170);
#1762=AXIS2_PLACEMENT_3D('',#2648,#2172,#2173);
#1763=AXIS2_PLACEMENT_3D('',#2650,#2174,#2175);
#1764=AXIS2_PLACEMENT_3D('',#2653,#2177,#2178);
#1765=AXIS2_PLACEMENT_3D('',#2654,#2179,#2180);
#1766=AXIS2_PLACEMENT_3D('',#2657,#2181,#2182);
#1767=AXIS2_PLACEMENT_3D('',#2661,#2184,#2185);
#1768=AXIS2_PLACEMENT_3D('',#2663,#2186,#2187);
#1769=AXIS2_PLACEMENT_3D('',#2665,#2188,#2189);
#1770=AXIS2_PLACEMENT_3D('',#2669,#2191,#2192);
#1771=AXIS2_PLACEMENT_3D('',#2673,#2194,#2195);
#1772=AXIS2_PLACEMENT_3D('',#2675,#2196,#2197);
#1773=AXIS2_PLACEMENT_3D('',#2677,#2198,#2199);
#1774=AXIS2_PLACEMENT_3D('',#2681,#2202,#2203);
#1775=AXIS2_PLACEMENT_3D('',#2683,#2204,#2205);
#1776=AXIS2_PLACEMENT_3D('',#2688,#2208,#2209);
#1777=AXIS2_PLACEMENT_3D('',#2690,#2210,#2211);
#1778=AXIS2_PLACEMENT_3D('',#2692,#2212,#2213);
#1779=AXIS2_PLACEMENT_3D('',#2696,#2215,#2216);
#1780=AXIS2_PLACEMENT_3D('',#2700,#2218,#2219);
#1781=AXIS2_PLACEMENT_3D('',#2702,#2220,#2221);
#1782=AXIS2_PLACEMENT_3D('',#2704,#2222,#2223);
#1783=AXIS2_PLACEMENT_3D('',#2706,#2225,#2226);
#1784=AXIS2_PLACEMENT_3D('',#2709,#2227,#2228);
#1785=AXIS2_PLACEMENT_3D('',#2713,#2230,#2231);
#1786=AXIS2_PLACEMENT_3D('',#2715,#2232,#2233);
#1787=AXIS2_PLACEMENT_3D('',#2717,#2234,#2235);
#1788=AXIS2_PLACEMENT_3D('',#2721,#2237,#2238);
#1789=AXIS2_PLACEMENT_3D('',#2725,#2240,#2241);
#1790=AXIS2_PLACEMENT_3D('',#2727,#2242,#2243);
#1791=AXIS2_PLACEMENT_3D('',#2729,#2244,#2245);
#1792=AXIS2_PLACEMENT_3D('',#2733,#2248,#2249);
#1793=AXIS2_PLACEMENT_3D('',#2735,#2250,#2251);
#1794=AXIS2_PLACEMENT_3D('',#2740,#2254,#2255);
#1795=AXIS2_PLACEMENT_3D('',#2742,#2256,#2257);
#1796=AXIS2_PLACEMENT_3D('',#2744,#2258,#2259);
#1797=AXIS2_PLACEMENT_3D('',#2748,#2261,#2262);
#1798=AXIS2_PLACEMENT_3D('',#2752,#2264,#2265);
#1799=AXIS2_PLACEMENT_3D('',#2754,#2266,#2267);
#1800=AXIS2_PLACEMENT_3D('',#2756,#2268,#2269);
#1801=AXIS2_PLACEMENT_3D('',#2758,#2271,#2272);
#1802=AXIS2_PLACEMENT_3D('',#2761,#2275,#2276);
#1803=AXIS2_PLACEMENT_3D('',#2763,#2278,#2279);
#1804=AXIS2_PLACEMENT_3D('',#2765,#2281,#2282);
#1805=AXIS2_PLACEMENT_3D('',#2767,#2284,#2285);
#1806=AXIS2_PLACEMENT_3D('',#2769,#2287,#2288);
#1807=AXIS2_PLACEMENT_3D('',#2771,#2290,#2291);
#1808=AXIS2_PLACEMENT_3D('',#2773,#2293,#2294);
#1809=AXIS2_PLACEMENT_3D('',#2775,#2296,#2297);
#1810=AXIS2_PLACEMENT_3D('',#2777,#2299,#2300);
#1811=AXIS2_PLACEMENT_3D('',#2779,#2302,#2303);
#1812=AXIS2_PLACEMENT_3D('',#2781,#2305,#2306);
#1813=AXIS2_PLACEMENT_3D('',#2782,#2307,#2308);
#1814=AXIS2_PLACEMENT_3D('',#2784,#2310,#2311);
#1815=AXIS2_PLACEMENT_3D('',#2785,#2312,#2313);
#1816=AXIS2_PLACEMENT_3D('',#2787,#2315,#2316);
#1817=AXIS2_PLACEMENT_3D('',#2788,#2317,#2318);
#1818=AXIS2_PLACEMENT_3D('',#2790,#2320,#2321);
#1819=AXIS2_PLACEMENT_3D('',#2792,#2323,#2324);
#1820=AXIS2_PLACEMENT_3D('',#2794,#2326,#2327);
#1821=AXIS2_PLACEMENT_3D('',#2796,#2329,#2330);
#1822=AXIS2_PLACEMENT_3D('',#2798,#2332,#2333);
#1823=AXIS2_PLACEMENT_3D('',#2800,#2335,#2336);
#1824=AXIS2_PLACEMENT_3D('',#2802,#2338,#2339);
#1825=AXIS2_PLACEMENT_3D('',#2804,#2341,#2342);
#1826=AXIS2_PLACEMENT_3D('',#2806,#2344,#2345);
#1827=AXIS2_PLACEMENT_3D('',#2808,#2347,#2348);
#1828=AXIS2_PLACEMENT_3D('',#2809,#2349,#2350);
#1829=AXIS2_PLACEMENT_3D('',#2810,#2351,#2352);
#1830=AXIS2_PLACEMENT_3D('',#2811,#2353,#2354);
#1831=AXIS2_PLACEMENT_3D('',#2813,#2355,#2356);
#1832=AXIS2_PLACEMENT_3D('',#2816,#2358,#2359);
#1833=AXIS2_PLACEMENT_3D('',#2817,#2360,#2361);
#1834=AXIS2_PLACEMENT_3D('',#2818,#2362,#2363);
#1835=AXIS2_PLACEMENT_3D('',#2819,#2364,#2365);
#1836=AXIS2_PLACEMENT_3D('',#2820,#2366,#2367);
#1837=AXIS2_PLACEMENT_3D('',#2821,#2368,#2369);
#1838=AXIS2_PLACEMENT_3D('',#2822,#2370,#2371);
#1839=AXIS2_PLACEMENT_3D('',#2823,#2372,#2373);
#1840=AXIS2_PLACEMENT_3D('',#2824,#2374,#2375);
#1841=DIRECTION('axis',(0.,0.,1.));
#1842=DIRECTION('refdir',(1.,0.,0.));
#1843=DIRECTION('axis',(0.,0.,1.));
#1844=DIRECTION('refdir',(1.,0.,0.));
#1845=DIRECTION('center_axis',(0.,1.,0.));
#1846=DIRECTION('ref_axis',(0.,0.,1.));
#1847=DIRECTION('center_axis',(0.,1.,0.));
#1848=DIRECTION('ref_axis',(0.,0.,1.));
#1849=DIRECTION('',(0.,1.,0.));
#1850=DIRECTION('center_axis',(0.,1.,0.));
#1851=DIRECTION('ref_axis',(0.,0.,1.));
#1852=DIRECTION('center_axis',(0.,1.,0.));
#1853=DIRECTION('ref_axis',(0.,0.,1.));
#1854=DIRECTION('center_axis',(0.,1.,0.));
#1855=DIRECTION('ref_axis',(0.,0.,1.));
#1856=DIRECTION('',(0.,1.,0.));
#1857=DIRECTION('center_axis',(0.,1.,0.));
#1858=DIRECTION('ref_axis',(0.,0.,1.));
#1859=DIRECTION('center_axis',(0.,1.,0.));
#1860=DIRECTION('ref_axis',(0.,0.,1.));
#1861=DIRECTION('center_axis',(0.,1.,0.));
#1862=DIRECTION('ref_axis',(0.,0.,1.));
#1863=DIRECTION('',(0.,1.,0.));
#1864=DIRECTION('center_axis',(0.,1.,0.));
#1865=DIRECTION('ref_axis',(0.,0.,1.));
#1866=DIRECTION('center_axis',(0.,1.,0.));
#1867=DIRECTION('ref_axis',(0.,0.,1.));
#1868=DIRECTION('center_axis',(0.,1.,0.));
#1869=DIRECTION('ref_axis',(0.,0.,1.));
#1870=DIRECTION('',(0.,1.,0.));
#1871=DIRECTION('center_axis',(0.,1.,0.));
#1872=DIRECTION('ref_axis',(0.,0.,1.));
#1873=DIRECTION('center_axis',(0.,1.,0.));
#1874=DIRECTION('ref_axis',(0.,0.,1.));
#1875=DIRECTION('center_axis',(0.,1.,0.));
#1876=DIRECTION('ref_axis',(0.,0.,1.));
#1877=DIRECTION('',(0.,1.,0.));
#1878=DIRECTION('center_axis',(0.,1.,0.));
#1879=DIRECTION('ref_axis',(0.,0.,1.));
#1880=DIRECTION('center_axis',(0.,0.,-1.));
#1881=DIRECTION('ref_axis',(-1.,0.,0.));
#1882=DIRECTION('',(0.,-1.,0.));
#1883=DIRECTION('',(-1.,0.,0.));
#1884=DIRECTION('',(0.,1.,0.));
#1885=DIRECTION('',(1.,0.,0.));
#1886=DIRECTION('center_axis',(-1.,0.,0.));
#1887=DIRECTION('ref_axis',(0.,0.,1.));
#1888=DIRECTION('',(0.,-1.,0.));
#1889=DIRECTION('',(0.,0.,1.));
#1890=DIRECTION('',(0.,1.,0.));
#1891=DIRECTION('',(0.,0.,-1.));
#1892=DIRECTION('center_axis',(0.,0.,-1.));
#1893=DIRECTION('ref_axis',(-1.,0.,0.));
#1894=DIRECTION('',(0.,-1.,0.));
#1895=DIRECTION('',(1.,0.,0.));
#1896=DIRECTION('',(0.,1.,0.));
#1897=DIRECTION('',(-1.,0.,0.));
#1898=DIRECTION('center_axis',(-1.,0.,0.));
#1899=DIRECTION('ref_axis',(0.,0.,1.));
#1900=DIRECTION('',(0.,1.,0.));
#1901=DIRECTION('',(0.,0.,1.));
#1902=DIRECTION('',(0.,-1.,0.));
#1903=DIRECTION('',(0.,0.,-1.));
#1904=DIRECTION('center_axis',(0.,1.,0.));
#1905=DIRECTION('ref_axis',(0.,0.,1.));
#1906=DIRECTION('',(0.,0.,1.));
#1907=DIRECTION('center_axis',(0.,1.,0.));
#1908=DIRECTION('ref_axis',(0.,0.,1.));
#1909=DIRECTION('',(1.,0.,0.));
#1910=DIRECTION('center_axis',(0.,1.,0.));
#1911=DIRECTION('ref_axis',(0.,0.,1.));
#1912=DIRECTION('',(0.,0.,-1.));
#1913=DIRECTION('center_axis',(0.,1.,0.));
#1914=DIRECTION('ref_axis',(0.,0.,1.));
#1915=DIRECTION('',(-1.,0.,0.));
#1916=DIRECTION('center_axis',(0.,1.,0.));
#1917=DIRECTION('ref_axis',(0.,0.,1.));
#1918=DIRECTION('center_axis',(0.,1.,0.));
#1919=DIRECTION('ref_axis',(0.,0.,1.));
#1920=DIRECTION('',(0.,0.,1.));
#1921=DIRECTION('center_axis',(0.,-1.,0.));
#1922=DIRECTION('ref_axis',(0.,0.,1.));
#1923=DIRECTION('',(-1.,0.,0.));
#1924=DIRECTION('center_axis',(0.,-1.,0.));
#1925=DIRECTION('ref_axis',(0.,0.,1.));
#1926=DIRECTION('',(0.,0.,-1.));
#1927=DIRECTION('center_axis',(0.,-1.,0.));
#1928=DIRECTION('ref_axis',(0.,0.,1.));
#1929=DIRECTION('',(1.,0.,0.));
#1930=DIRECTION('center_axis',(0.,-1.,0.));
#1931=DIRECTION('ref_axis',(0.,0.,1.));
#1932=DIRECTION('center_axis',(0.,1.,0.));
#1933=DIRECTION('ref_axis',(0.,0.,1.));
#1934=DIRECTION('center_axis',(0.,1.,0.));
#1935=DIRECTION('ref_axis',(0.,0.,1.));
#1936=DIRECTION('center_axis',(0.,-1.,0.));
#1937=DIRECTION('ref_axis',(0.,0.,1.));
#1938=DIRECTION('center_axis',(0.,-1.,0.));
#1939=DIRECTION('ref_axis',(0.,0.,-1.));
#1940=DIRECTION('center_axis',(0.,1.,0.));
#1941=DIRECTION('ref_axis',(0.,0.,1.));
#1942=DIRECTION('center_axis',(0.,-1.,0.));
#1943=DIRECTION('ref_axis',(0.,0.,1.));
#1944=DIRECTION('center_axis',(0.,1.,0.));
#1945=DIRECTION('ref_axis',(0.,0.,1.));
#1946=DIRECTION('center_axis',(0.,1.,0.));
#1947=DIRECTION('ref_axis',(0.,0.,1.));
#1948=DIRECTION('center_axis',(0.,-1.,0.));
#1949=DIRECTION('ref_axis',(0.,0.,1.));
#1950=DIRECTION('center_axis',(0.,-1.,0.));
#1951=DIRECTION('ref_axis',(0.,0.,-1.));
#1952=DIRECTION('center_axis',(0.,1.,0.));
#1953=DIRECTION('ref_axis',(0.,0.,1.));
#1954=DIRECTION('center_axis',(0.,-1.,0.));
#1955=DIRECTION('ref_axis',(0.,0.,1.));
#1956=DIRECTION('center_axis',(0.,1.,0.));
#1957=DIRECTION('ref_axis',(0.,0.,1.));
#1958=DIRECTION('center_axis',(0.,0.,1.));
#1959=DIRECTION('ref_axis',(1.,0.,0.));
#1960=DIRECTION('center_axis',(1.,0.,0.));
#1961=DIRECTION('ref_axis',(0.,0.,-1.));
#1962=DIRECTION('center_axis',(-1.,0.,0.));
#1963=DIRECTION('ref_axis',(0.,0.,1.));
#1964=DIRECTION('center_axis',(1.,0.,0.));
#1965=DIRECTION('ref_axis',(0.,0.,-1.));
#1966=DIRECTION('center_axis',(0.,0.,1.));
#1967=DIRECTION('ref_axis',(1.,0.,0.));
#1968=DIRECTION('center_axis',(0.,0.,1.));
#1969=DIRECTION('ref_axis',(1.,0.,0.));
#1970=DIRECTION('center_axis',(0.,1.,0.));
#1971=DIRECTION('ref_axis',(0.,0.,1.));
#1972=DIRECTION('center_axis',(0.,0.,1.));
#1973=DIRECTION('ref_axis',(1.,0.,0.));
#1974=DIRECTION('center_axis',(0.,1.,0.));
#1975=DIRECTION('ref_axis',(0.,0.,1.));
#1976=DIRECTION('center_axis',(1.,0.,0.));
#1977=DIRECTION('ref_axis',(0.,0.,-1.));
#1978=DIRECTION('center_axis',(0.,0.,-1.));
#1979=DIRECTION('ref_axis',(-1.,0.,0.));
#1980=DIRECTION('center_axis',(0.,0.,1.));
#1981=DIRECTION('ref_axis',(1.,0.,0.));
#1982=DIRECTION('center_axis',(1.,0.,0.));
#1983=DIRECTION('ref_axis',(0.,0.,-1.));
#1984=DIRECTION('center_axis',(1.,0.,0.));
#1985=DIRECTION('ref_axis',(0.,0.,-1.));
#1986=DIRECTION('center_axis',(0.,1.,0.));
#1987=DIRECTION('ref_axis',(0.,0.,1.));
#1988=DIRECTION('center_axis',(0.,1.,0.));
#1989=DIRECTION('ref_axis',(0.,0.,1.));
#1990=DIRECTION('center_axis',(0.,0.,1.));
#1991=DIRECTION('ref_axis',(1.,0.,0.));
#1992=DIRECTION('center_axis',(-1.,0.,0.));
#1993=DIRECTION('ref_axis',(0.,0.,1.));
#1994=DIRECTION('center_axis',(1.,0.,0.));
#1995=DIRECTION('ref_axis',(0.,0.,-1.));
#1996=DIRECTION('center_axis',(-1.,0.,0.));
#1997=DIRECTION('ref_axis',(0.,0.,1.));
#1998=DIRECTION('center_axis',(0.,0.,1.));
#1999=DIRECTION('ref_axis',(1.,0.,0.));
#2000=DIRECTION('center_axis',(0.,0.,1.));
#2001=DIRECTION('ref_axis',(1.,0.,0.));
#2002=DIRECTION('center_axis',(0.,1.,0.));
#2003=DIRECTION('ref_axis',(0.,0.,1.));
#2004=DIRECTION('center_axis',(0.,0.,1.));
#2005=DIRECTION('ref_axis',(1.,0.,0.));
#2006=DIRECTION('center_axis',(0.,1.,0.));
#2007=DIRECTION('ref_axis',(0.,0.,1.));
#2008=DIRECTION('center_axis',(-1.,0.,0.));
#2009=DIRECTION('ref_axis',(0.,0.,1.));
#2010=DIRECTION('center_axis',(0.,0.,-1.));
#2011=DIRECTION('ref_axis',(-1.,0.,0.));
#2012=DIRECTION('center_axis',(0.,0.,1.));
#2013=DIRECTION('ref_axis',(1.,0.,0.));
#2014=DIRECTION('center_axis',(-1.,0.,0.));
#2015=DIRECTION('ref_axis',(0.,0.,1.));
#2016=DIRECTION('center_axis',(-1.,0.,0.));
#2017=DIRECTION('ref_axis',(0.,0.,1.));
#2018=DIRECTION('center_axis',(0.,1.,0.));
#2019=DIRECTION('ref_axis',(0.,0.,1.));
#2020=DIRECTION('center_axis',(0.,1.,0.));
#2021=DIRECTION('ref_axis',(0.,0.,1.));
#2022=DIRECTION('axis',(0.,0.,1.));
#2023=DIRECTION('refdir',(1.,0.,0.));
#2024=DIRECTION('center_axis',(0.,1.,0.));
#2025=DIRECTION('ref_axis',(0.,0.,1.));
#2026=DIRECTION('center_axis',(0.,1.,0.));
#2027=DIRECTION('ref_axis',(0.,0.,1.));
#2028=DIRECTION('',(0.,1.,0.));
#2029=DIRECTION('center_axis',(0.,1.,0.));
#2030=DIRECTION('ref_axis',(0.,0.,1.));
#2031=DIRECTION('center_axis',(0.,1.,0.));
#2032=DIRECTION('ref_axis',(0.,0.,1.));
#2033=DIRECTION('center_axis',(0.,1.,0.));
#2034=DIRECTION('ref_axis',(0.,0.,1.));
#2035=DIRECTION('center_axis',(-1.,0.,0.));
#2036=DIRECTION('ref_axis',(0.,0.,-1.));
#2037=DIRECTION('center_axis',(0.,-1.,0.));
#2038=DIRECTION('ref_axis',(0.,0.,1.));
#2039=DIRECTION('center_axis',(0.,-1.,0.));
#2040=DIRECTION('ref_axis',(0.,0.,1.));
#2041=DIRECTION('center_axis',(0.,-1.,0.));
#2042=DIRECTION('ref_axis',(0.,0.,-1.));
#2043=DIRECTION('center_axis',(0.,1.,0.));
#2044=DIRECTION('ref_axis',(0.,0.,1.));
#2045=DIRECTION('',(0.,1.,0.));
#2046=DIRECTION('center_axis',(0.,1.,0.));
#2047=DIRECTION('ref_axis',(-1.38777878078145E-17,0.,1.));
#2048=DIRECTION('center_axis',(0.,1.,0.));
#2049=DIRECTION('ref_axis',(-1.38777878078145E-17,0.,1.));
#2050=DIRECTION('axis',(0.,0.,1.));
#2051=DIRECTION('refdir',(1.,0.,0.));
#2052=DIRECTION('center_axis',(-5.42341872339446E-30,1.,2.7856650715617E-30));
#2053=DIRECTION('ref_axis',(1.51078281062137E-59,-2.7856650715617E-30,1.));
#2054=DIRECTION('center_axis',(-5.42341872339446E-30,1.,2.7856650715617E-30));
#2055=DIRECTION('ref_axis',(2.8681187888985E-59,-2.7856650715617E-30,1.));
#2056=DIRECTION('',(-5.42341872339446E-30,1.,2.7856650715617E-30));
#2057=DIRECTION('center_axis',(-5.42341872339446E-30,1.,2.7856650715617E-30));
#2058=DIRECTION('ref_axis',(1.51078281062137E-59,-2.7856650715617E-30,1.));
#2059=DIRECTION('center_axis',(-5.42341872339446E-30,1.,2.7856650715617E-30));
#2060=DIRECTION('ref_axis',(1.51078281062137E-59,-2.7856650715617E-30,1.));
#2061=DIRECTION('center_axis',(-5.42341872339446E-30,1.,2.7856650715617E-30));
#2062=DIRECTION('ref_axis',(3.02156562124273E-59,-2.7856650715617E-30,1.));
#2063=DIRECTION('',(-5.42341872339446E-30,1.,2.7856650715617E-30));
#2064=DIRECTION('center_axis',(-5.42341872339446E-30,1.,2.7856650715617E-30));
#2065=DIRECTION('ref_axis',(1.51078281062137E-59,-2.7856650715617E-30,1.));
#2066=DIRECTION('center_axis',(-5.42341872339446E-30,1.,2.7856650715617E-30));
#2067=DIRECTION('ref_axis',(1.51078281062137E-59,-2.7856650715617E-30,1.));
#2068=DIRECTION('center_axis',(-5.42341872339446E-30,1.,2.7856650715617E-30));
#2069=DIRECTION('ref_axis',(3.02156562124273E-59,-2.7856650715617E-30,1.));
#2070=DIRECTION('',(-5.42341872339446E-30,1.,2.7856650715617E-30));
#2071=DIRECTION('center_axis',(-5.42341872339446E-30,1.,2.7856650715617E-30));
#2072=DIRECTION('ref_axis',(1.51078281062137E-59,-2.7856650715617E-30,1.));
#2073=DIRECTION('center_axis',(-5.42341872339446E-30,1.,2.7856650715617E-30));
#2074=DIRECTION('ref_axis',(1.51078281062137E-59,-2.7856650715617E-30,1.));
#2075=DIRECTION('center_axis',(-5.42341872339446E-30,1.,2.7856650715617E-30));
#2076=DIRECTION('ref_axis',(3.02156562124273E-59,-2.7856650715617E-30,1.));
#2077=DIRECTION('',(-5.42341872339446E-30,1.,2.7856650715617E-30));
#2078=DIRECTION('center_axis',(-5.42341872339446E-30,1.,2.7856650715617E-30));
#2079=DIRECTION('ref_axis',(1.51078281062137E-59,-2.7856650715617E-30,1.));
#2080=DIRECTION('center_axis',(-5.42341872339446E-30,1.,2.7856650715617E-30));
#2081=DIRECTION('ref_axis',(1.51078281062137E-59,-2.7856650715617E-30,1.));
#2082=DIRECTION('center_axis',(-5.42341872339446E-30,1.,2.7856650715617E-30));
#2083=DIRECTION('ref_axis',(3.02156562124273E-59,-2.7856650715617E-30,1.));
#2084=DIRECTION('',(-5.42341872339446E-30,1.,2.7856650715617E-30));
#2085=DIRECTION('center_axis',(-5.42341872339446E-30,1.,2.7856650715617E-30));
#2086=DIRECTION('ref_axis',(1.51078281062137E-59,-2.7856650715617E-30,1.));
#2087=DIRECTION('center_axis',(-5.42341872339446E-30,1.,2.7856650715617E-30));
#2088=DIRECTION('ref_axis',(1.51078281062137E-59,-2.7856650715617E-30,1.));
#2089=DIRECTION('center_axis',(-5.42341872339446E-30,1.,2.7856650715617E-30));
#2090=DIRECTION('ref_axis',(3.02156562124273E-59,-2.7856650715617E-30,1.));
#2091=DIRECTION('',(-5.42341872339446E-30,1.,2.7856650715617E-30));
#2092=DIRECTION('center_axis',(-5.42341872339446E-30,1.,2.7856650715617E-30));
#2093=DIRECTION('ref_axis',(1.51078281062137E-59,-2.7856650715617E-30,1.));
#2094=DIRECTION('center_axis',(-5.42341872339446E-30,1.,2.7856650715617E-30));
#2095=DIRECTION('ref_axis',(0.,0.,1.));
#2096=DIRECTION('center_axis',(-5.42341872339446E-30,1.,2.7856650715617E-30));
#2097=DIRECTION('ref_axis',(1.51078281062137E-59,-2.7856650715617E-30,1.));
#2098=DIRECTION('center_axis',(-1.,-5.42341872339446E-30,1.64477485129653E-16));
#2099=DIRECTION('ref_axis',(-1.64477485129653E-16,0.,-1.));
#2100=DIRECTION('center_axis',(5.42341872339446E-30,-1.,-2.7856650715617E-30));
#2101=DIRECTION('ref_axis',(1.51078281062137E-59,-2.7856650715617E-30,1.));
#2102=DIRECTION('center_axis',(-5.42341872339446E-30,1.,3.00753220115511E-30));
#2103=DIRECTION('ref_axis',(1.63111064509564E-59,-3.00753220115511E-30,
1.));
#2104=DIRECTION('center_axis',(-5.42341872339446E-30,1.,2.7856650715617E-30));
#2105=DIRECTION('ref_axis',(3.02156562124273E-59,-2.7856650715617E-30,1.));
#2106=DIRECTION('',(-5.42341872339446E-30,1.,3.00753220115511E-30));
#2107=DIRECTION('center_axis',(-5.42341872339446E-30,1.,2.7856650715617E-30));
#2108=DIRECTION('ref_axis',(3.73969860926369E-17,0.,1.));
#2109=DIRECTION('center_axis',(-5.42341872339446E-30,1.,2.7856650715617E-30));
#2110=DIRECTION('ref_axis',(3.71063845128728E-17,-2.7856650715617E-30,1.));
#2111=DIRECTION('center_axis',(-1.,-5.42341872339446E-30,1.63611814155286E-16));
#2112=DIRECTION('ref_axis',(-1.63611814155286E-16,0.,-1.));
#2113=DIRECTION('center_axis',(5.42341872339446E-30,-1.,-2.7856650715617E-30));
#2114=DIRECTION('ref_axis',(3.65204942310906E-17,-2.7856650715617E-30,1.));
#2115=DIRECTION('center_axis',(5.42341872339446E-30,-1.,-2.7856650715617E-30));
#2116=DIRECTION('ref_axis',(3.65204942310906E-17,-2.7856650715617E-30,1.));
#2117=DIRECTION('center_axis',(5.42341872339446E-30,-1.,-2.7856650715617E-30));
#2118=DIRECTION('ref_axis',(-3.65204942310906E-17,2.7856650715617E-30,-1.));
#2119=DIRECTION('center_axis',(-5.42341872339446E-30,1.,2.7856650715617E-30));
#2120=DIRECTION('ref_axis',(3.65204942310906E-17,-2.7856650715617E-30,1.));
#2121=DIRECTION('',(-5.42341872339446E-30,1.,2.7856650715617E-30));
#2122=DIRECTION('center_axis',(-5.42341872339446E-30,1.,-2.78566507156169E-30));
#2123=DIRECTION('ref_axis',(2.77555756156288E-17,2.78566507156169E-30,1.));
#2124=DIRECTION('center_axis',(-5.42341872339446E-30,1.,-2.78566507156169E-30));
#2125=DIRECTION('ref_axis',(2.77555756156288E-17,2.78566507156169E-30,1.));
#2126=DIRECTION('axis',(0.,0.,1.));
#2127=DIRECTION('refdir',(1.,0.,0.));
#2128=DIRECTION('center_axis',(0.,-1.,0.));
#2129=DIRECTION('ref_axis',(-5.55111512312576E-17,0.,-1.));
#2130=DIRECTION('center_axis',(0.,1.,0.));
#2131=DIRECTION('ref_axis',(5.55111512312576E-17,0.,1.));
#2132=DIRECTION('',(0.,1.,0.));
#2133=DIRECTION('center_axis',(0.,1.,0.));
#2134=DIRECTION('ref_axis',(5.55111512312576E-17,0.,1.));
#2135=DIRECTION('center_axis',(0.,1.,0.));
#2136=DIRECTION('ref_axis',(5.55111512312576E-17,0.,1.));
#2137=DIRECTION('center_axis',(0.,1.,0.));
#2138=DIRECTION('ref_axis',(5.55111512312576E-17,0.,1.));
#2139=DIRECTION('axis',(0.,0.,1.));
#2140=DIRECTION('refdir',(1.,0.,0.));
#2141=DIRECTION('center_axis',(2.61947219093537E-16,1.,-5.05688216913818E-17));
#2142=DIRECTION('ref_axis',(-1.10981324742611E-16,5.05688216913819E-17,
1.));
#2143=DIRECTION('center_axis',(2.61947219093537E-16,1.,-5.05688216913818E-17));
#2144=DIRECTION('ref_axis',(-1.10981324742611E-16,5.05688216913819E-17,
1.));
#2145=DIRECTION('',(2.61947219093537E-16,1.,-5.05688216913818E-17));
#2146=DIRECTION('center_axis',(2.61947219093537E-16,1.,-5.05688216913818E-17));
#2147=DIRECTION('ref_axis',(-1.10981324742611E-16,5.05688216913819E-17,
1.));
#2148=DIRECTION('center_axis',(-2.61947219093537E-16,-1.,5.05688216913818E-17));
#2149=DIRECTION('ref_axis',(-1.32463622148944E-32,-5.05688216913818E-17,
-1.));
#2150=DIRECTION('center_axis',(-2.61947219093537E-16,-1.,5.05688216913818E-17));
#2151=DIRECTION('ref_axis',(1.32463622148944E-32,5.05688216913818E-17,1.));
#2152=DIRECTION('',(-2.61947219093537E-16,-1.,5.05688216913818E-17));
#2153=DIRECTION('center_axis',(-2.61947219093537E-16,-1.,5.05688216913818E-17));
#2154=DIRECTION('ref_axis',(2.64927244297885E-32,5.05688216913818E-17,1.));
#2155=DIRECTION('',(-2.61947219093537E-16,-1.,5.05688216913818E-17));
#2156=DIRECTION('center_axis',(-2.61947219093537E-16,-1.,5.05688216913818E-17));
#2157=DIRECTION('ref_axis',(1.10981324742611E-16,-5.05688216913819E-17,
-1.));
#2158=DIRECTION('center_axis',(-2.61947219093537E-16,-1.,5.05688216913818E-17));
#2159=DIRECTION('ref_axis',(1.10981324742611E-16,-5.05688216913819E-17,
-1.));
#2160=DIRECTION('',(-2.61947219093537E-16,-1.,5.05688216913818E-17));
#2161=DIRECTION('center_axis',(-2.61947219093537E-16,-1.,5.05688216913818E-17));
#2162=DIRECTION('ref_axis',(1.10981324742611E-16,-5.05688216913819E-17,
-1.));
#2163=DIRECTION('',(-2.61947219093537E-16,-1.,5.05688216913818E-17));
#2164=DIRECTION('center_axis',(-2.61947219093537E-16,-1.,5.05688216913818E-17));
#2165=DIRECTION('ref_axis',(-1.32463622148944E-32,-5.05688216913818E-17,
-1.));
#2166=DIRECTION('center_axis',(-2.61947219093537E-16,-1.,5.05688216913818E-17));
#2167=DIRECTION('ref_axis',(1.32463622148944E-32,5.05688216913818E-17,1.));
#2168=DIRECTION('',(-2.61947219093537E-16,-1.,5.05688216913818E-17));
#2169=DIRECTION('center_axis',(-2.61947219093537E-16,-1.,5.05688216913818E-17));
#2170=DIRECTION('ref_axis',(2.64927244297889E-32,5.05688216913818E-17,1.));
#2171=DIRECTION('',(-2.61947219093537E-16,-1.,5.05688216913818E-17));
#2172=DIRECTION('center_axis',(-2.61947219093537E-16,-1.,5.05688216913818E-17));
#2173=DIRECTION('ref_axis',(1.09761749745439E-16,-5.05688216913819E-17,
-1.));
#2174=DIRECTION('center_axis',(-2.61947219093537E-16,-1.,5.05688216913818E-17));
#2175=DIRECTION('ref_axis',(-1.88729230812297E-15,5.05688216913823E-17,
1.));
#2176=DIRECTION('',(-2.61947219093537E-16,-1.,5.05688216913819E-17));
#2177=DIRECTION('center_axis',(-2.61947219093537E-16,-1.,5.05688216913818E-17));
#2178=DIRECTION('ref_axis',(1.09761749745439E-16,-5.05688216913819E-17,
-1.));
#2179=DIRECTION('center_axis',(2.61947219093537E-16,1.,5.0568821691382E-17));
#2180=DIRECTION('ref_axis',(-1.11022302462516E-16,-5.0568821691382E-17,
1.));
#2181=DIRECTION('center_axis',(-2.61947219093537E-16,-1.,5.05688216913818E-17));
#2182=DIRECTION('ref_axis',(-1.12329276055274E-16,5.05688216913819E-17,
1.));
#2183=DIRECTION('',(1.11022302462516E-16,5.0568821691382E-17,-1.));
#2184=DIRECTION('center_axis',(2.61947219093537E-16,1.,-5.05688216913818E-17));
#2185=DIRECTION('ref_axis',(-1.12242473919644E-16,5.05688216913819E-17,
1.));
#2186=DIRECTION('center_axis',(-2.61947219093537E-16,-1.,5.05688216913818E-17));
#2187=DIRECTION('ref_axis',(-1.82123199577618E-16,5.05688216913819E-17,
1.));
#2188=DIRECTION('center_axis',(2.61947219093537E-16,1.,-5.05688216913818E-17));
#2189=DIRECTION('ref_axis',(-3.00472787334257E-32,-5.05688216913818E-17,
-1.));
#2190=DIRECTION('',(0.951056516295154,2.33499984356149E-16,0.309016994374947));
#2191=DIRECTION('center_axis',(-2.61947219093537E-16,-1.,5.05688216913818E-17));
#2192=DIRECTION('ref_axis',(1.32463622148944E-32,5.05688216913818E-17,1.));
#2193=DIRECTION('',(-0.951056516295154,-2.33499984356149E-16,-0.309016994374947));
#2194=DIRECTION('center_axis',(2.61947219093537E-16,1.,-5.05688216913818E-17));
#2195=DIRECTION('ref_axis',(3.00472787334257E-32,5.05688216913818E-17,1.));
#2196=DIRECTION('center_axis',(-2.61947219093537E-16,-1.,5.05688216913818E-17));
#2197=DIRECTION('ref_axis',(-2.5173028630338E-32,-5.05688216913818E-17,
-1.));
#2198=DIRECTION('center_axis',(2.61947219093537E-16,1.,-5.05688216913818E-17));
#2199=DIRECTION('ref_axis',(-3.00472787334257E-32,-5.05688216913818E-17,
-1.));
#2200=DIRECTION('',(0.587785252292473,1.94879748396051E-16,-0.809016994374948));
#2201=DIRECTION('',(-0.587785252292473,-1.94879748396051E-16,0.809016994374947));
#2202=DIRECTION('center_axis',(2.61947219093537E-16,1.,-5.05688216913818E-17));
#2203=DIRECTION('ref_axis',(3.00472787334257E-32,5.05688216913818E-17,1.));
#2204=DIRECTION('center_axis',(2.61947219093537E-16,1.,-5.05688216913818E-17));
#2205=DIRECTION('ref_axis',(-3.00472787334257E-32,-5.05688216913818E-17,
-1.));
#2206=DIRECTION('',(-0.587785252292473,-1.13057676128363E-16,-0.809016994374947));
#2207=DIRECTION('',(0.587785252292473,1.13057676128363E-16,0.809016994374947));
#2208=DIRECTION('center_axis',(2.61947219093537E-16,1.,-5.05688216913818E-17));
#2209=DIRECTION('ref_axis',(3.00472787334257E-32,5.05688216913818E-17,1.));
#2210=DIRECTION('center_axis',(-2.61947219093537E-16,-1.,5.05688216913818E-17));
#2211=DIRECTION('ref_axis',(-2.5173028630338E-32,-5.05688216913818E-17,
-1.));
#2212=DIRECTION('center_axis',(2.61947219093537E-16,1.,-5.05688216913818E-17));
#2213=DIRECTION('ref_axis',(-3.00472787334257E-32,-5.05688216913818E-17,
-1.));
#2214=DIRECTION('',(-0.951056516295154,-2.64753234932456E-16,0.309016994374947));
#2215=DIRECTION('center_axis',(-2.61947219093537E-16,-1.,5.05688216913818E-17));
#2216=DIRECTION('ref_axis',(1.32463622148944E-32,5.05688216913818E-17,1.));
#2217=DIRECTION('',(0.951056516295154,2.64753234932456E-16,-0.309016994374947));
#2218=DIRECTION('center_axis',(2.61947219093537E-16,1.,-5.05688216913818E-17));
#2219=DIRECTION('ref_axis',(3.00472787334257E-32,5.05688216913818E-17,1.));
#2220=DIRECTION('center_axis',(-2.61947219093537E-16,-1.,5.05688216913818E-17));
#2221=DIRECTION('ref_axis',(1.82123199577618E-16,-5.05688216913819E-17,
-1.));
#2222=DIRECTION('center_axis',(2.61947219093537E-16,1.,-5.05688216913818E-17));
#2223=DIRECTION('ref_axis',(1.12242473919644E-16,-5.05688216913819E-17,
-1.));
#2224=DIRECTION('',(-1.11022302462516E-16,-5.0568821691382E-17,1.));
#2225=DIRECTION('center_axis',(2.61947219093537E-16,1.,5.0568821691382E-17));
#2226=DIRECTION('ref_axis',(-1.11022302462516E-16,-5.0568821691382E-17,
1.));
#2227=DIRECTION('center_axis',(-2.61947219093537E-16,-1.,5.05688216913818E-17));
#2228=DIRECTION('ref_axis',(-1.12329276055274E-16,5.05688216913819E-17,
1.));
#2229=DIRECTION('',(-1.11022302462516E-16,-5.0568821691382E-17,1.));
#2230=DIRECTION('center_axis',(2.61947219093537E-16,1.,-5.05688216913818E-17));
#2231=DIRECTION('ref_axis',(1.12242473919644E-16,-5.05688216913819E-17,
-1.));
#2232=DIRECTION('center_axis',(-2.61947219093537E-16,-1.,5.05688216913818E-17));
#2233=DIRECTION('ref_axis',(1.82123199577618E-16,-5.05688216913819E-17,
-1.));
#2234=DIRECTION('center_axis',(2.61947219093537E-16,1.,-5.05688216913818E-17));
#2235=DIRECTION('ref_axis',(2.64927244297889E-32,5.05688216913818E-17,1.));
#2236=DIRECTION('',(0.951056516295154,2.64753234932456E-16,-0.309016994374947));
#2237=DIRECTION('center_axis',(-2.61947219093537E-16,-1.,5.05688216913818E-17));
#2238=DIRECTION('ref_axis',(2.64927244297892E-32,5.05688216913818E-17,1.));
#2239=DIRECTION('',(-0.951056516295154,-2.64753234932456E-16,0.309016994374947));
#2240=DIRECTION('center_axis',(2.61947219093537E-16,1.,-5.05688216913818E-17));
#2241=DIRECTION('ref_axis',(-2.64927244297889E-32,-5.05688216913818E-17,
-1.));
#2242=DIRECTION('center_axis',(-2.61947219093537E-16,-1.,5.05688216913818E-17));
#2243=DIRECTION('ref_axis',(-2.64927244297889E-32,-5.05688216913818E-17,
-1.));
#2244=DIRECTION('center_axis',(2.61947219093537E-16,1.,-5.05688216913818E-17));
#2245=DIRECTION('ref_axis',(2.64927244297889E-32,5.05688216913818E-17,1.));
#2246=DIRECTION('',(0.587785252292473,1.13057676128363E-16,0.809016994374947));
#2247=DIRECTION('',(-0.587785252292473,-1.13057676128363E-16,-0.809016994374947));
#2248=DIRECTION('center_axis',(2.61947219093537E-16,1.,-5.05688216913818E-17));
#2249=DIRECTION('ref_axis',(-2.64927244297889E-32,-5.05688216913818E-17,
-1.));
#2250=DIRECTION('center_axis',(2.61947219093537E-16,1.,-5.05688216913818E-17));
#2251=DIRECTION('ref_axis',(2.64927244297889E-32,5.05688216913818E-17,1.));
#2252=DIRECTION('',(-0.587785252292473,-1.94879748396051E-16,0.809016994374947));
#2253=DIRECTION('',(0.587785252292473,1.94879748396051E-16,-0.809016994374948));
#2254=DIRECTION('center_axis',(2.61947219093537E-16,1.,-5.05688216913818E-17));
#2255=DIRECTION('ref_axis',(-2.64927244297889E-32,-5.05688216913818E-17,
-1.));
#2256=DIRECTION('center_axis',(-2.61947219093537E-16,-1.,5.05688216913818E-17));
#2257=DIRECTION('ref_axis',(-2.64927244297889E-32,-5.05688216913818E-17,
-1.));
#2258=DIRECTION('center_axis',(2.61947219093537E-16,1.,-5.05688216913818E-17));
#2259=DIRECTION('ref_axis',(2.64927244297889E-32,5.05688216913818E-17,1.));
#2260=DIRECTION('',(-0.951056516295154,-2.33499984356149E-16,-0.309016994374947));
#2261=DIRECTION('center_axis',(-2.61947219093537E-16,-1.,5.05688216913818E-17));
#2262=DIRECTION('ref_axis',(2.64927244297889E-32,5.05688216913818E-17,1.));
#2263=DIRECTION('',(0.951056516295154,2.33499984356149E-16,0.309016994374947));
#2264=DIRECTION('center_axis',(2.61947219093537E-16,1.,-5.05688216913818E-17));
#2265=DIRECTION('ref_axis',(-2.64927244297889E-32,-5.05688216913818E-17,
-1.));
#2266=DIRECTION('center_axis',(-2.61947219093537E-16,-1.,5.05688216913818E-17));
#2267=DIRECTION('ref_axis',(-1.82123199577618E-16,5.05688216913819E-17,
1.));
#2268=DIRECTION('center_axis',(2.61947219093537E-16,1.,-5.05688216913818E-17));
#2269=DIRECTION('ref_axis',(-1.12242473919644E-16,5.05688216913819E-17,
1.));
#2270=DIRECTION('',(1.11022302462516E-16,5.0568821691382E-17,-1.));
#2271=DIRECTION('center_axis',(-2.61947219093537E-16,-1.,5.05688216913818E-17));
#2272=DIRECTION('ref_axis',(4.6195413228266E-14,5.05688216913697E-17,1.));
#2273=DIRECTION('',(-2.61947219093537E-16,-1.,5.05688216913818E-17));
#2274=DIRECTION('',(-2.61947219093537E-16,-1.,5.05688216913818E-17));
#2275=DIRECTION('center_axis',(-1.,-2.61947219093537E-16,-1.11022302462516E-16));
#2276=DIRECTION('ref_axis',(-1.11022302462516E-16,-5.0568821691382E-17,
1.));
#2277=DIRECTION('',(-2.61947219093537E-16,-1.,5.05688216913818E-17));
#2278=DIRECTION('center_axis',(-2.61947219093537E-16,-1.,5.05688216913818E-17));
#2279=DIRECTION('ref_axis',(1.12242473919644E-16,-5.05688216913819E-17,
-1.));
#2280=DIRECTION('',(-2.61947219093537E-16,-1.,5.05688216913818E-17));
#2281=DIRECTION('center_axis',(-2.61947219093537E-16,-1.,5.05688216913818E-17));
#2282=DIRECTION('ref_axis',(1.82123199577618E-16,-5.05688216913819E-17,
-1.));
#2283=DIRECTION('',(-2.61947219093537E-16,-1.,5.05688216913818E-17));
#2284=DIRECTION('center_axis',(-2.61947219093537E-16,-1.,5.05688216913818E-17));
#2285=DIRECTION('ref_axis',(-3.00472787334257E-32,-5.05688216913818E-17,
-1.));
#2286=DIRECTION('',(-2.61947219093537E-16,-1.,5.05688216913818E-17));
#2287=DIRECTION('center_axis',(0.309016994374947,1.29039949720116E-16,-0.951056516295154));
#2288=DIRECTION('ref_axis',(-0.951056516295154,-2.33499984356149E-16,-0.309016994374947));
#2289=DIRECTION('',(-2.61947219093537E-16,-1.,5.05688216913818E-17));
#2290=DIRECTION('center_axis',(-2.61947219093537E-16,-1.,5.05688216913818E-17));
#2291=DIRECTION('ref_axis',(0.95105651629515,-2.33499984356148E-16,0.309016994374957));
#2292=DIRECTION('',(-2.61947219093537E-16,-1.,5.05688216913818E-17));
#2293=DIRECTION('center_axis',(-0.309016994374947,-1.29039949720117E-16,
0.951056516295154));
#2294=DIRECTION('ref_axis',(0.951056516295154,2.33499984356149E-16,0.309016994374947));
#2295=DIRECTION('',(-2.61947219093537E-16,-1.,5.05688216913818E-17));
#2296=DIRECTION('center_axis',(-2.61947219093537E-16,-1.,5.05688216913818E-17));
#2297=DIRECTION('ref_axis',(-3.00472787334257E-32,-5.05688216913818E-17,
-1.));
#2298=DIRECTION('',(-2.61947219093537E-16,-1.,5.05688216913818E-17));
#2299=DIRECTION('center_axis',(-2.61947219093537E-16,-1.,5.05688216913818E-17));
#2300=DIRECTION('ref_axis',(-2.5173028630338E-32,-5.05688216913818E-17,
-1.));
#2301=DIRECTION('',(-2.61947219093537E-16,-1.,5.05688216913818E-17));
#2302=DIRECTION('center_axis',(-2.61947219093537E-16,-1.,5.05688216913818E-17));
#2303=DIRECTION('ref_axis',(-3.00472787334257E-32,-5.05688216913818E-17,
-1.));
#2304=DIRECTION('',(-2.61947219093537E-16,-1.,5.05688216913818E-17));
#2305=DIRECTION('center_axis',(-0.809016994374948,-1.82196144259928E-16,
-0.587785252292473));
#2306=DIRECTION('ref_axis',(-0.587785252292473,-1.94879748396051E-16,0.809016994374948));
#2307=DIRECTION('center_axis',(0.809016994374948,1.82196144259928E-16,0.587785252292473));
#2308=DIRECTION('ref_axis',(0.587785252292473,1.94879748396051E-16,-0.809016994374948));
#2309=DIRECTION('',(-2.61947219093537E-16,-1.,5.05688216913818E-17));
#2310=DIRECTION('center_axis',(-2.61947219093537E-16,-1.,5.05688216913818E-17));
#2311=DIRECTION('ref_axis',(-3.00472787334257E-32,-5.05688216913818E-17,
-1.));
#2312=DIRECTION('center_axis',(-2.61947219093537E-16,-1.,5.05688216913818E-17));
#2313=DIRECTION('ref_axis',(-3.00472787334257E-32,-5.05688216913818E-17,
-1.));
#2314=DIRECTION('',(-2.61947219093537E-16,-1.,5.05688216913818E-17));
#2315=DIRECTION('center_axis',(-0.809016994374947,-2.41643359491932E-16,
0.587785252292473));
#2316=DIRECTION('ref_axis',(0.587785252292473,1.13057676128362E-16,0.809016994374948));
#2317=DIRECTION('center_axis',(0.809016994374947,2.41643359491932E-16,-0.587785252292473));
#2318=DIRECTION('ref_axis',(-0.587785252292473,-1.13057676128362E-16,-0.809016994374947));
#2319=DIRECTION('',(-2.61947219093537E-16,-1.,5.05688216913818E-17));
#2320=DIRECTION('center_axis',(-2.61947219093537E-16,-1.,5.05688216913818E-17));
#2321=DIRECTION('ref_axis',(-3.00472787334257E-32,-5.05688216913818E-17,
-1.));
#2322=DIRECTION('',(-2.61947219093537E-16,-1.,5.05688216913818E-17));
#2323=DIRECTION('center_axis',(-2.61947219093537E-16,-1.,5.05688216913818E-17));
#2324=DIRECTION('ref_axis',(-2.5173028630338E-32,-5.05688216913818E-17,
-1.));
#2325=DIRECTION('',(-2.61947219093537E-16,-1.,5.05688216913818E-17));
#2326=DIRECTION('center_axis',(-2.61947219093537E-16,-1.,5.05688216913818E-17));
#2327=DIRECTION('ref_axis',(-3.00472787334257E-32,-5.05688216913818E-17,
-1.));
#2328=DIRECTION('',(-2.61947219093537E-16,-1.,5.05688216913818E-17));
#2329=DIRECTION('center_axis',(0.309016994374947,3.28523349382053E-17,0.951056516295154));
#2330=DIRECTION('ref_axis',(0.951056516295154,2.64753234932456E-16,-0.309016994374947));
#2331=DIRECTION('',(-2.61947219093537E-16,-1.,5.05688216913818E-17));
#2332=DIRECTION('center_axis',(-2.61947219093537E-16,-1.,5.05688216913818E-17));
#2333=DIRECTION('ref_axis',(-0.951056516295152,2.64753234932456E-16,0.309016994374953));
#2334=DIRECTION('',(-2.61947219093537E-16,-1.,5.05688216913818E-17));
#2335=DIRECTION('center_axis',(-0.309016994374947,-3.28523349382053E-17,
-0.951056516295154));
#2336=DIRECTION('ref_axis',(-0.951056516295154,-2.64753234932456E-16,0.309016994374947));
#2337=DIRECTION('',(-2.61947219093537E-16,-1.,5.05688216913818E-17));
#2338=DIRECTION('center_axis',(-2.61947219093537E-16,-1.,5.05688216913818E-17));
#2339=DIRECTION('ref_axis',(-3.00472787334257E-32,-5.05688216913818E-17,
-1.));
#2340=DIRECTION('',(-2.61947219093537E-16,-1.,5.05688216913818E-17));
#2341=DIRECTION('center_axis',(-2.61947219093537E-16,-1.,5.05688216913818E-17));
#2342=DIRECTION('ref_axis',(1.82123199577618E-16,-5.05688216913819E-17,
-1.));
#2343=DIRECTION('',(-2.61947219093537E-16,-1.,5.05688216913818E-17));
#2344=DIRECTION('center_axis',(-2.61947219093537E-16,-1.,5.05688216913818E-17));
#2345=DIRECTION('ref_axis',(1.12242473919644E-16,-5.05688216913819E-17,
-1.));
#2346=DIRECTION('',(-2.61947219093537E-16,-1.,5.05688216913818E-17));
#2347=DIRECTION('center_axis',(1.,2.61947219093537E-16,1.11022302462516E-16));
#2348=DIRECTION('ref_axis',(1.11022302462516E-16,5.0568821691382E-17,-1.));
#2349=DIRECTION('center_axis',(2.61947219093537E-16,1.,5.0568821691382E-17));
#2350=DIRECTION('ref_axis',(-1.11022302462516E-16,-5.0568821691382E-17,
1.));
#2351=DIRECTION('axis',(0.,0.,1.));
#2352=DIRECTION('refdir',(1.,0.,0.));
#2353=DIRECTION('center_axis',(0.,-1.,0.));
#2354=DIRECTION('ref_axis',(0.,0.,-1.));
#2355=DIRECTION('center_axis',(0.,1.,0.));
#2356=DIRECTION('ref_axis',(0.,0.,1.));
#2357=DIRECTION('',(0.,1.,0.));
#2358=DIRECTION('center_axis',(0.,1.,0.));
#2359=DIRECTION('ref_axis',(0.,0.,1.));
#2360=DIRECTION('center_axis',(0.,1.,0.));
#2361=DIRECTION('ref_axis',(0.,0.,1.));
#2362=DIRECTION('center_axis',(0.,1.,0.));
#2363=DIRECTION('ref_axis',(0.,0.,1.));
#2364=DIRECTION('',(0.,0.,1.));
#2365=DIRECTION('',(1.,0.,0.));
#2366=DIRECTION('',(0.125564112476647,0.,0.992085507231081));
#2367=DIRECTION('',(0.992085507231081,0.,-0.125564112476647));
#2368=DIRECTION('',(0.968580795826003,-4.70256415486959E-16,0.248699099228498));
#2369=DIRECTION('',(0.248699099228498,6.5691704770049E-16,-0.968580795826003));
#2370=DIRECTION('',(-0.478342044496565,0.,0.878173609525386));
#2371=DIRECTION('',(0.878173609525386,0.,0.478342044496565));
#2372=DIRECTION('',(-0.314013180355799,-6.30625751921208E-16,0.949418623454815));
#2373=DIRECTION('',(0.949418623454815,-4.76435157199843E-16,0.314013180355799));
#2374=DIRECTION('',(0.,0.,1.));
#2375=DIRECTION('',(1.,0.,0.));
#2376=CARTESIAN_POINT('',(0.,0.,0.));
#2377=CARTESIAN_POINT('',(0.,0.,0.));
#2378=CARTESIAN_POINT('Origin',(88.4184469844746,20.,-2074.54745691296));
#2379=CARTESIAN_POINT('',(88.4184469844746,20.,-2087.04745691296));
#2380=CARTESIAN_POINT('Origin',(88.4184469844746,20.,-2074.54745691296));
#2381=CARTESIAN_POINT('',(88.4184469844746,30.,-2087.04745691296));
#2382=CARTESIAN_POINT('',(88.4184469844746,20.,-2087.04745691296));
#2383=CARTESIAN_POINT('Origin',(88.4184469844746,30.,-2074.54745691296));
#2384=CARTESIAN_POINT('Origin',(-16.5815530155254,30.,-1969.54745691296));
#2385=CARTESIAN_POINT('',(-16.5815530155254,0.,-1977.54745691296));
#2386=CARTESIAN_POINT('Origin',(-16.5815530155254,0.,-1969.54745691296));
#2387=CARTESIAN_POINT('',(-16.5815530155254,30.,-1977.54745691296));
#2388=CARTESIAN_POINT('',(-16.5815530155254,30.,-1977.54745691296));
#2389=CARTESIAN_POINT('Origin',(-16.5815530155254,30.,-1969.54745691296));
#2390=CARTESIAN_POINT('Origin',(-16.5815530155254,30.,-2179.54745691296));
#2391=CARTESIAN_POINT('',(-16.5815530155254,0.,-2187.54745691296));
#2392=CARTESIAN_POINT('Origin',(-16.5815530155254,0.,-2179.54745691296));
#2393=CARTESIAN_POINT('',(-16.5815530155254,30.,-2187.54745691296));
#2394=CARTESIAN_POINT('',(-16.5815530155254,30.,-2187.54745691296));
#2395=CARTESIAN_POINT('Origin',(-16.5815530155254,30.,-2179.54745691296));
#2396=CARTESIAN_POINT('Origin',(193.418446984475,30.,-2179.54745691296));
#2397=CARTESIAN_POINT('',(193.418446984475,0.,-2187.54745691296));
#2398=CARTESIAN_POINT('Origin',(193.418446984475,0.,-2179.54745691296));
#2399=CARTESIAN_POINT('',(193.418446984475,30.,-2187.54745691296));
#2400=CARTESIAN_POINT('',(193.418446984475,30.,-2187.54745691296));
#2401=CARTESIAN_POINT('Origin',(193.418446984475,30.,-2179.54745691296));
#2402=CARTESIAN_POINT('Origin',(193.418446984475,30.,-1969.54745691296));
#2403=CARTESIAN_POINT('',(193.418446984475,0.,-1977.54745691296));
#2404=CARTESIAN_POINT('Origin',(193.418446984475,0.,-1969.54745691296));
#2405=CARTESIAN_POINT('',(193.418446984475,30.,-1977.54745691296));
#2406=CARTESIAN_POINT('',(193.418446984475,30.,-1977.54745691296));
#2407=CARTESIAN_POINT('Origin',(193.418446984475,30.,-1969.54745691296));
#2408=CARTESIAN_POINT('Origin',(-36.5815530155254,30.,-2199.54745691296));
#2409=CARTESIAN_POINT('',(193.418446984475,28.5,-2199.54745691296));
#2410=CARTESIAN_POINT('',(193.418446984475,1.5,-2199.54745691296));
#2411=CARTESIAN_POINT('',(193.418446984475,0.,-2199.54745691296));
#2412=CARTESIAN_POINT('',(-16.5815530155254,1.5,-2199.54745691296));
#2413=CARTESIAN_POINT('',(-16.5815530155254,1.5,-2199.54745691296));
#2414=CARTESIAN_POINT('',(-16.5815530155254,28.5,-2199.54745691296));
#2415=CARTESIAN_POINT('',(-16.5815530155254,30.,-2199.54745691296));
#2416=CARTESIAN_POINT('',(-36.5815530155254,28.5,-2199.54745691296));
#2417=CARTESIAN_POINT('Origin',(-36.5815530155254,30.,-1949.54745691296));
#2418=CARTESIAN_POINT('',(-36.5815530155254,28.5,-2179.54745691296));
#2419=CARTESIAN_POINT('',(-36.5815530155254,1.5,-2179.54745691296));
#2420=CARTESIAN_POINT('',(-36.5815530155254,30.,-2179.54745691296));
#2421=CARTESIAN_POINT('',(-36.5815530155254,1.5,-1969.54745691296));
#2422=CARTESIAN_POINT('',(-36.5815530155254,1.5,-1969.54745691296));
#2423=CARTESIAN_POINT('',(-36.5815530155254,28.5,-1969.54745691296));
#2424=CARTESIAN_POINT('',(-36.5815530155254,30.,-1969.54745691296));
#2425=CARTESIAN_POINT('',(-36.5815530155254,28.5,-1949.54745691296));
#2426=CARTESIAN_POINT('Origin',(-36.5815530155254,30.,-1949.54745691296));
#2427=CARTESIAN_POINT('',(-16.5815530155254,28.5,-1949.54745691296));
#2428=CARTESIAN_POINT('',(-16.5815530155254,1.5,-1949.54745691296));
#2429=CARTESIAN_POINT('',(-16.5815530155254,0.,-1949.54745691296));
#2430=CARTESIAN_POINT('',(193.418446984475,1.5,-1949.54745691296));
#2431=CARTESIAN_POINT('',(-36.5815530155254,1.5,-1949.54745691296));
#2432=CARTESIAN_POINT('',(193.418446984475,28.5,-1949.54745691296));
#2433=CARTESIAN_POINT('',(193.418446984475,30.,-1949.54745691296));
#2434=CARTESIAN_POINT('',(-16.5815530155254,28.5,-1949.54745691296));
#2435=CARTESIAN_POINT('Origin',(213.418446984475,30.,-1949.54745691296));
#2436=CARTESIAN_POINT('',(213.418446984475,1.5,-2179.54745691296));
#2437=CARTESIAN_POINT('',(213.418446984475,28.5,-2179.54745691296));
#2438=CARTESIAN_POINT('',(213.418446984475,30.,-2179.54745691296));
#2439=CARTESIAN_POINT('',(213.418446984475,28.5,-1969.54745691296));
#2440=CARTESIAN_POINT('',(213.418446984475,28.5,-1969.54745691296));
#2441=CARTESIAN_POINT('',(213.418446984475,1.5,-1969.54745691296));
#2442=CARTESIAN_POINT('',(213.418446984475,30.,-1969.54745691296));
#2443=CARTESIAN_POINT('',(213.418446984475,1.5,-1949.54745691296));
#2444=CARTESIAN_POINT('Origin',(0.,30.,0.));
#2445=CARTESIAN_POINT('',(-35.0815530155254,30.,-2179.54745691296));
#2446=CARTESIAN_POINT('',(-35.0815530155254,30.,-1969.54745691296));
#2447=CARTESIAN_POINT('',(-35.0815530155254,30.,0.));
#2448=CARTESIAN_POINT('',(-16.5815530155254,30.,-1951.04745691296));
#2449=CARTESIAN_POINT('Origin',(-16.5815530155254,30.,-1969.54745691296));
#2450=CARTESIAN_POINT('',(193.418446984475,30.,-1951.04745691296));
#2451=CARTESIAN_POINT('',(193.418446984475,30.,-1951.04745691296));
#2452=CARTESIAN_POINT('',(211.918446984475,30.,-1969.54745691296));
#2453=CARTESIAN_POINT('Origin',(193.418446984475,30.,-1969.54745691296));
#2454=CARTESIAN_POINT('',(211.918446984475,30.,-2179.54745691296));
#2455=CARTESIAN_POINT('',(211.918446984475,30.,-2179.54745691296));
#2456=CARTESIAN_POINT('',(193.418446984475,30.,-2198.04745691296));
#2457=CARTESIAN_POINT('Origin',(193.418446984475,30.,-2179.54745691296));
#2458=CARTESIAN_POINT('',(-16.5815530155254,30.,-2198.04745691296));
#2459=CARTESIAN_POINT('',(0.,30.,-2198.04745691296));
#2460=CARTESIAN_POINT('Origin',(-16.5815530155254,30.,-2179.54745691296));
#2461=CARTESIAN_POINT('Origin',(0.,0.,0.));
#2462=CARTESIAN_POINT('',(211.918446984475,0.,-2179.54745691296));
#2463=CARTESIAN_POINT('',(211.918446984475,0.,-1969.54745691296));
#2464=CARTESIAN_POINT('',(211.918446984475,0.,0.));
#2465=CARTESIAN_POINT('',(193.418446984475,0.,-1951.04745691296));
#2466=CARTESIAN_POINT('Origin',(193.418446984475,0.,-1969.54745691296));
#2467=CARTESIAN_POINT('',(-16.5815530155254,0.,-1951.04745691296));
#2468=CARTESIAN_POINT('',(0.,0.,-1951.04745691296));
#2469=CARTESIAN_POINT('',(-35.0815530155254,0.,-1969.54745691296));
#2470=CARTESIAN_POINT('Origin',(-16.5815530155254,0.,-1969.54745691296));
#2471=CARTESIAN_POINT('',(-35.0815530155254,0.,-2179.54745691296));
#2472=CARTESIAN_POINT('',(-35.0815530155254,0.,-2179.54745691296));
#2473=CARTESIAN_POINT('',(-16.5815530155254,0.,-2198.04745691296));
#2474=CARTESIAN_POINT('Origin',(-16.5815530155254,0.,-2179.54745691296));
#2475=CARTESIAN_POINT('',(193.418446984475,0.,-2198.04745691296));
#2476=CARTESIAN_POINT('',(193.418446984475,0.,-2198.04745691296));
#2477=CARTESIAN_POINT('Origin',(193.418446984475,0.,-2179.54745691296));
#2478=CARTESIAN_POINT('Origin',(-16.5815530155254,30.,-1969.54745691296));
#2479=CARTESIAN_POINT('Origin',(-16.5815530155254,1.5,-1969.54745691296));
#2480=CARTESIAN_POINT('Origin',(-16.5815530155254,28.5,-1969.54745691296));
#2481=CARTESIAN_POINT('Origin',(-16.5815530155254,30.,-2179.54745691296));
#2482=CARTESIAN_POINT('Origin',(-16.5815530155254,1.5,-2179.54745691296));
#2483=CARTESIAN_POINT('Origin',(-16.5815530155254,28.5,-2179.54745691296));
#2484=CARTESIAN_POINT('Origin',(193.418446984475,30.,-2179.54745691296));
#2485=CARTESIAN_POINT('Origin',(193.418446984475,1.5,-2179.54745691296));
#2486=CARTESIAN_POINT('Origin',(193.418446984475,28.5,-2179.54745691296));
#2487=CARTESIAN_POINT('Origin',(193.418446984475,30.,-1969.54745691296));
#2488=CARTESIAN_POINT('Origin',(193.418446984475,1.5,-1969.54745691296));
#2489=CARTESIAN_POINT('Origin',(193.418446984475,28.5,-1969.54745691296));
#2490=CARTESIAN_POINT('Origin',(-16.5815530155254,1.5,-2179.54745691296));
#2491=CARTESIAN_POINT('Origin',(-35.0815530155254,1.5,-2179.54745691296));
#2492=CARTESIAN_POINT('Origin',(-16.5815530155254,1.5,-2198.04745691296));
#2493=CARTESIAN_POINT('Origin',(0.,1.5,-2198.04745691296));
#2494=CARTESIAN_POINT('Origin',(193.418446984475,1.5,-2198.04745691296));
#2495=CARTESIAN_POINT('Origin',(-35.0815530155254,1.5,0.));
#2496=CARTESIAN_POINT('Origin',(-35.0815530155254,1.5,-1969.54745691296));
#2497=CARTESIAN_POINT('Origin',(193.418446984475,1.5,-2179.54745691296));
#2498=CARTESIAN_POINT('Origin',(211.918446984475,1.5,-2179.54745691296));
#2499=CARTESIAN_POINT('Origin',(-16.5815530155254,1.5,-1969.54745691296));
#2500=CARTESIAN_POINT('Origin',(-16.5815530155254,1.5,-1951.04745691296));
#2501=CARTESIAN_POINT('Origin',(211.918446984475,1.5,-1949.54745691296));
#2502=CARTESIAN_POINT('Origin',(211.918446984475,1.5,-1969.54745691296));
#2503=CARTESIAN_POINT('Origin',(-36.5815530155254,1.5,-1951.04745691296));
#2504=CARTESIAN_POINT('Origin',(193.418446984475,1.5,-1951.04745691296));
#2505=CARTESIAN_POINT('Origin',(193.418446984475,1.5,-1969.54745691296));
#2506=CARTESIAN_POINT('Origin',(193.418446984475,28.5,-2179.54745691296));
#2507=CARTESIAN_POINT('Origin',(211.918446984475,28.5,-2179.54745691296));
#2508=CARTESIAN_POINT('Origin',(193.418446984475,28.5,-2198.04745691296));
#2509=CARTESIAN_POINT('Origin',(-36.5815530155254,28.5,-2198.04745691296));
#2510=CARTESIAN_POINT('Origin',(-16.5815530155254,28.5,-2198.04745691296));
#2511=CARTESIAN_POINT('Origin',(211.918446984475,28.5,0.));
#2512=CARTESIAN_POINT('Origin',(211.918446984475,28.5,-1969.54745691296));
#2513=CARTESIAN_POINT('Origin',(-16.5815530155254,28.5,-2179.54745691296));
#2514=CARTESIAN_POINT('Origin',(-35.0815530155254,28.5,-2179.54745691296));
#2515=CARTESIAN_POINT('Origin',(193.418446984475,28.5,-1969.54745691296));
#2516=CARTESIAN_POINT('Origin',(193.418446984475,28.5,-1951.04745691296));
#2517=CARTESIAN_POINT('Origin',(-35.0815530155254,28.5,-1949.54745691296));
#2518=CARTESIAN_POINT('Origin',(-35.0815530155254,28.5,-1969.54745691296));
#2519=CARTESIAN_POINT('Origin',(0.,28.5,-1951.04745691296));
#2520=CARTESIAN_POINT('Origin',(-16.5815530155254,28.5,-1951.04745691296));
#2521=CARTESIAN_POINT('Origin',(-16.5815530155254,28.5,-1969.54745691296));
#2522=CARTESIAN_POINT('Origin',(88.4184469844746,20.,-2074.54745691296));
#2523=CARTESIAN_POINT('',(0.,0.,0.));
#2524=CARTESIAN_POINT('Origin',(296.23500439103,-43.,-495.721631563692));
#2525=CARTESIAN_POINT('',(296.23500439103,0.,-508.221631563692));
#2526=CARTESIAN_POINT('Origin',(296.23500439103,0.,-495.721631563692));
#2527=CARTESIAN_POINT('',(296.23500439103,17.,-508.221631563692));
#2528=CARTESIAN_POINT('',(296.23500439103,-43.,-508.221631563692));
#2529=CARTESIAN_POINT('Origin',(296.23500439103,17.,-495.721631563692));
#2530=CARTESIAN_POINT('Origin',(296.235004391031,15.5,-495.721631563692));
#2531=CARTESIAN_POINT('',(296.235004391031,17.,-601.721631563692));
#2532=CARTESIAN_POINT('Origin',(296.235004391031,17.,-495.721631563692));
#2533=CARTESIAN_POINT('',(296.235004391031,15.5,-603.221631563692));
#2534=CARTESIAN_POINT('Origin',(296.235004391031,15.5,-601.721631563692));
#2535=CARTESIAN_POINT('',(296.235004391031,15.5,-388.221631563692));
#2536=CARTESIAN_POINT('Origin',(296.235004391031,15.5,-495.721631563692));
#2537=CARTESIAN_POINT('Origin',(296.235004391031,15.5,-495.721631563692));
#2538=CARTESIAN_POINT('Origin',(296.235004391031,17.,-495.721631563692));
#2539=CARTESIAN_POINT('',(296.235004391031,2.22044604925031E-15,-388.221631563692));
#2540=CARTESIAN_POINT('Origin',(296.235004391031,0.,-495.721631563692));
#2541=CARTESIAN_POINT('',(296.235004391031,17.,-388.221631563692));
#2542=CARTESIAN_POINT('Origin',(296.235004391031,17.,-495.721631563692));
#2543=CARTESIAN_POINT('Origin',(296.235004391031,0.,-495.721631563692));
#2544=CARTESIAN_POINT('',(0.,0.,0.));
#2545=CARTESIAN_POINT('Origin',(97.46416980426,17.,303.733119632278));
#2546=CARTESIAN_POINT('',(97.46416980426,4.88498130835069E-14,298.808119632278));
#2547=CARTESIAN_POINT('Origin',(97.46416980426,4.85722573273506E-14,303.733119632278));
#2548=CARTESIAN_POINT('',(97.46416980426,17.,298.808119632278));
#2549=CARTESIAN_POINT('',(97.46416980426,17.,298.808119632278));
#2550=CARTESIAN_POINT('Origin',(97.46416980426,17.,303.733119632278));
#2551=CARTESIAN_POINT('Origin',(-59.9821245185343,17.,303.733119632278));
#2552=CARTESIAN_POINT('',(-59.9821245185343,0.,298.808119632278));
#2553=CARTESIAN_POINT('Origin',(-59.9821245185343,0.,303.733119632278));
#2554=CARTESIAN_POINT('',(-59.9821245185343,17.,298.808119632278));
#2555=CARTESIAN_POINT('',(-59.9821245185343,17.,298.808119632278));
#2556=CARTESIAN_POINT('Origin',(-59.9821245185343,17.,303.733119632278));
#2557=CARTESIAN_POINT('Origin',(18.741022642863,17.,283.733119632278));
#2558=CARTESIAN_POINT('',(18.741022642863,0.,280.233119632278));
#2559=CARTESIAN_POINT('Origin',(18.7410226428626,0.,283.733119632278));
#2560=CARTESIAN_POINT('',(18.741022642863,17.,280.233119632278));
#2561=CARTESIAN_POINT('',(18.741022642863,17.,280.233119632278));
#2562=CARTESIAN_POINT('Origin',(18.741022642863,17.,283.733119632278));
#2563=CARTESIAN_POINT('Origin',(38.7410226428653,17.,303.733119632278));
#2564=CARTESIAN_POINT('',(38.7410226428653,0.,300.233119632278));
#2565=CARTESIAN_POINT('Origin',(38.7410226428657,0.,303.733119632278));
#2566=CARTESIAN_POINT('',(38.7410226428653,17.,300.233119632278));
#2567=CARTESIAN_POINT('',(38.7410226428653,17.,300.233119632278));
#2568=CARTESIAN_POINT('Origin',(38.7410226428653,17.,303.733119632278));
#2569=CARTESIAN_POINT('Origin',(18.7410226428626,17.,323.733119632279));
#2570=CARTESIAN_POINT('',(18.7410226428626,0.,320.233119632279));
#2571=CARTESIAN_POINT('Origin',(18.7410226428626,0.,323.733119632278));
#2572=CARTESIAN_POINT('',(18.7410226428626,17.,320.233119632279));
#2573=CARTESIAN_POINT('',(18.7410226428626,17.,320.233119632279));
#2574=CARTESIAN_POINT('Origin',(18.7410226428626,17.,323.733119632279));
#2575=CARTESIAN_POINT('Origin',(-1.25897735713698,17.,303.733119632279));
#2576=CARTESIAN_POINT('',(-1.25897735713698,0.,300.233119632279));
#2577=CARTESIAN_POINT('Origin',(-1.25897735713698,0.,303.733119632279));
#2578=CARTESIAN_POINT('',(-1.25897735713698,17.,300.233119632279));
#2579=CARTESIAN_POINT('',(-1.25897735713698,17.,300.233119632279));
#2580=CARTESIAN_POINT('Origin',(-1.25897735713698,17.,303.733119632279));
#2581=CARTESIAN_POINT('Origin',(18.7410226428648,16.5,303.733119632278));
#2582=CARTESIAN_POINT('',(18.7410226428648,16.5,291.233119632278));
#2583=CARTESIAN_POINT('Origin',(18.7410226428648,16.5,303.733119632278));
#2584=CARTESIAN_POINT('',(18.7410226428648,17.,290.733119632278));
#2585=CARTESIAN_POINT('Origin',(18.7410226428648,16.5,290.733119632278));
#2586=CARTESIAN_POINT('Origin',(18.7410226428648,17.,303.733119632278));
#2587=CARTESIAN_POINT('Origin',(18.7410226428644,-73.,303.733119632278));
#2588=CARTESIAN_POINT('',(18.7410226428644,0.,291.233119632278));
#2589=CARTESIAN_POINT('Origin',(18.7410226428644,0.,303.733119632278));
#2590=CARTESIAN_POINT('',(18.7410226428644,-73.,291.233119632278));
#2591=CARTESIAN_POINT('Origin',(18.7410226428648,15.5,303.733119632278));
#2592=CARTESIAN_POINT('',(18.7410226428648,17.,210.233119632278));
#2593=CARTESIAN_POINT('Origin',(18.7410226428648,17.,303.733119632278));
#2594=CARTESIAN_POINT('',(18.7410226428648,15.5,208.733119632278));
#2595=CARTESIAN_POINT('Origin',(18.7410226428648,15.5,210.233119632278));
#2596=CARTESIAN_POINT('',(18.7410226428648,15.5,398.733119632278));
#2597=CARTESIAN_POINT('Origin',(18.7410226428648,15.5,303.733119632278));
#2598=CARTESIAN_POINT('Origin',(18.7410226428648,15.5,303.733119632278));
#2599=CARTESIAN_POINT('Origin',(18.7410226428648,17.,303.733119632278));
#2600=CARTESIAN_POINT('',(18.7410226428648,-2.22044604925031E-15,398.733119632279));
#2601=CARTESIAN_POINT('Origin',(18.7410226428644,0.,303.733119632278));
#2602=CARTESIAN_POINT('',(18.7410226428648,17.,398.733119632279));
#2603=CARTESIAN_POINT('Origin',(18.7410226428648,17.,303.733119632278));
#2604=CARTESIAN_POINT('Origin',(18.7410226428644,0.,303.733119632278));
#2605=CARTESIAN_POINT('',(0.,0.,0.));
#2606=CARTESIAN_POINT('Origin',(0.,40.,0.));
#2607=CARTESIAN_POINT('',(-3.23385543541199E-16,0.,4.83000000000002));
#2608=CARTESIAN_POINT('Origin',(0.,0.,0.));
#2609=CARTESIAN_POINT('',(-3.23385543541199E-16,40.,4.83000000000002));
#2610=CARTESIAN_POINT('',(-3.23385543541199E-16,40.,4.83000000000002));
#2611=CARTESIAN_POINT('Origin',(0.,40.,0.));
#2612=CARTESIAN_POINT('Origin',(0.,40.,0.));
#2613=CARTESIAN_POINT('Origin',(0.,0.,0.));
#2614=CARTESIAN_POINT('',(0.,0.,0.));
#2615=CARTESIAN_POINT('Origin',(0.196389981728107,9.52499999999995,14.3245422672531));
#2616=CARTESIAN_POINT('',(0.196389981728107,9.52499999999995,1.62454226725312));
#2617=CARTESIAN_POINT('Origin',(0.196389981728107,9.52499999999995,14.3245422672531));
#2618=CARTESIAN_POINT('',(0.196389981728107,12.6999999999999,1.62454226725311));
#2619=CARTESIAN_POINT('',(0.196389981728107,9.52499999999995,1.62454226725312));
#2620=CARTESIAN_POINT('Origin',(0.196389981728107,12.6999999999999,14.3245422672531));
#2621=CARTESIAN_POINT('Origin',(29.1600960736921,12.7000000000002,54.1896636820751));
#2622=CARTESIAN_POINT('',(25.2557800588381,12.7,57.0263153096353));
#2623=CARTESIAN_POINT('',(33.0644120885452,12.7000000000002,51.3530120545092));
#2624=CARTESIAN_POINT('Origin',(29.1600960736921,12.7000000000002,54.1896636820751));
#2625=CARTESIAN_POINT('',(25.2557800588381,0.,57.0263153096353));
#2626=CARTESIAN_POINT('',(25.2557800588381,12.7,57.0263153096353));
#2627=CARTESIAN_POINT('',(33.0644120885454,1.66533453693773E-13,51.3530120545087));
#2628=CARTESIAN_POINT('Origin',(29.1600960736921,1.66533453693773E-13,54.1896636820751));
#2629=CARTESIAN_POINT('',(33.0644120885452,12.7000000000002,51.3530120545092));
#2630=CARTESIAN_POINT('Origin',(0.196389981727885,12.6999999999999,154.439874761711));
#2631=CARTESIAN_POINT('',(-44.54372429145,12.6999999999999,92.7571204877404));
#2632=CARTESIAN_POINT('',(44.9365042549055,12.7000000000001,92.7571204877395));
#2633=CARTESIAN_POINT('Origin',(0.196389981727885,12.6999999999999,154.439874761711));
#2634=CARTESIAN_POINT('',(-44.54372429145,-5.55111512312578E-14,92.7571204877404));
#2635=CARTESIAN_POINT('',(-44.54372429145,12.6999999999999,92.7571204877404));
#2636=CARTESIAN_POINT('',(44.9365042549055,1.11022302462516E-13,92.7571204877395));
#2637=CARTESIAN_POINT('Origin',(0.196389981727996,-5.55111512312578E-14,
154.439874761711));
#2638=CARTESIAN_POINT('',(44.9365042549055,12.7000000000001,92.7571204877395));
#2639=CARTESIAN_POINT('Origin',(-28.767316110236,12.6999999999999,54.1896636820724));
#2640=CARTESIAN_POINT('',(-32.6716321250896,12.7,51.35301205451));
#2641=CARTESIAN_POINT('',(-24.8630000953821,12.7000000000001,57.0263153096384));
#2642=CARTESIAN_POINT('Origin',(-28.767316110236,12.6999999999999,54.1896636820724));
#2643=CARTESIAN_POINT('',(-32.6716321250895,0.,51.3530120545105));
#2644=CARTESIAN_POINT('',(-32.6716321250896,12.7,51.35301205451));
#2645=CARTESIAN_POINT('',(-24.8630000953821,1.11022302462516E-13,57.0263153096384));
#2646=CARTESIAN_POINT('Origin',(-28.767316110236,0.,54.1896636820724));
#2647=CARTESIAN_POINT('',(-24.8630000953821,12.7000000000001,57.0263153096384));
#2648=CARTESIAN_POINT('Origin',(0.196389981728107,59.182,14.3245422672531));
#2649=CARTESIAN_POINT('',(0.196389981728092,9.52499999999995,23.2145422672531));
#2650=CARTESIAN_POINT('Origin',(0.196389981728107,9.52499999999995,14.3245422672531));
#2651=CARTESIAN_POINT('',(0.196389981728089,-6.21724893790088E-14,23.2145422672531));
#2652=CARTESIAN_POINT('',(0.196389981728105,59.182,23.2145422672531));
#2653=CARTESIAN_POINT('Origin',(0.196389981728107,-5.55111512312578E-14,
14.3245422672531));
#2654=CARTESIAN_POINT('Origin',(0.196389981728107,12.7,-34.9514577327463));
#2655=CARTESIAN_POINT('',(5.02238998172821,12.7,-34.9514577327463));
#2656=CARTESIAN_POINT('',(-4.62961001827178,12.7,-34.9514577327459));
#2657=CARTESIAN_POINT('Origin',(0.196389981728107,12.7,-34.9514577327463));
#2658=CARTESIAN_POINT('',(-4.62961001827222,12.7000000000002,-76.5025437375311));
#2659=CARTESIAN_POINT('',(-4.62961001827178,12.7,-34.9514577327459));
#2660=CARTESIAN_POINT('',(-9.70961001827242,12.7000000000001,-75.4263257814172));
#2661=CARTESIAN_POINT('Origin',(-1.59000334476855,12.7000000000001,-49.6273886803462));
#2662=CARTESIAN_POINT('',(-82.1006355728287,12.6999999999999,-22.8311670701098));
#2663=CARTESIAN_POINT('Origin',(-82.1613360785705,12.6999999999999,-99.0311428932596));
#2664=CARTESIAN_POINT('',(-84.6939860043709,12.6999999999999,-18.332369605421));
#2665=CARTESIAN_POINT('Origin',(-60.07348477912,12.7000000000001,-7.13665223247828));
#2666=CARTESIAN_POINT('',(-45.1765549003784,12.7,-5.4923778952074));
#2667=CARTESIAN_POINT('',(-45.1765549003784,12.7,-5.4923778952074));
#2668=CARTESIAN_POINT('',(-48.1591869300858,12.7,3.68721960007434));
#2669=CARTESIAN_POINT('Origin',(-46.6678709152318,12.7,-0.902579147566751));
#2670=CARTESIAN_POINT('',(-87.6766180340772,12.6999999999999,-9.15277211013876));
#2671=CARTESIAN_POINT('',(-48.1591869300858,12.7,3.68721960007434));
#2672=CARTESIAN_POINT('',(-88.2228802653845,12.6999999999999,-3.98883536926853));
#2673=CARTESIAN_POINT('Origin',(-61.17753657217,12.7000000000001,-3.73873020481819));
#2674=CARTESIAN_POINT('',(-60.5719689840063,12.7000000000001,81.1119190693219));
#2675=CARTESIAN_POINT('Origin',(-133.061210019987,12.7,57.6225611805379));
#2676=CARTESIAN_POINT('',(-57.0947476954385,12.7000000000001,84.9685467671164));
#2677=CARTESIAN_POINT('Origin',(-38.8388344446712,12.7000000000001,65.0127255748467));
#2678=CARTESIAN_POINT('',(-32.6716321250896,12.7,51.35301205451));
#2679=CARTESIAN_POINT('',(-49.2861156657315,12.7,90.6418500222435));
#2680=CARTESIAN_POINT('',(-24.8630000953821,12.7000000000001,57.0263153096384));
#2681=CARTESIAN_POINT('Origin',(-35.9483893251246,12.7000000000001,67.1127568790628));
#2682=CARTESIAN_POINT('',(49.6788956291876,12.7000000000001,90.6418500222421));
#2683=CARTESIAN_POINT('Origin',(36.3411692885806,12.7000000000002,67.1127568790633));
#2684=CARTESIAN_POINT('',(25.2557800588381,12.7,57.0263153096353));
#2685=CARTESIAN_POINT('',(57.4875276588944,12.7000000000001,84.9685467671164));
#2686=CARTESIAN_POINT('',(33.0644120885452,12.7000000000002,51.3530120545092));
#2687=CARTESIAN_POINT('',(60.964748947462,12.7000000000002,81.1119190693224));
#2688=CARTESIAN_POINT('Origin',(39.2316144081271,12.7000000000002,65.0127255748485));
#2689=CARTESIAN_POINT('',(88.61566022884,12.7,-3.98883536926897));
#2690=CARTESIAN_POINT('Origin',(133.453989983443,12.7,57.6225611805374));
#2691=CARTESIAN_POINT('',(88.0693979975334,12.7,-9.15277211014009));
#2692=CARTESIAN_POINT('Origin',(61.5703165356259,12.7000000000001,-3.73873020481819));
#2693=CARTESIAN_POINT('',(48.5519668935416,12.7000000000002,3.6872196000739));
#2694=CARTESIAN_POINT('',(48.5519668935416,12.7000000000002,3.6872196000739));
#2695=CARTESIAN_POINT('',(45.5693348638345,12.7000000000002,-5.49237789520696));
#2696=CARTESIAN_POINT('Origin',(47.0606508786874,12.7000000000001,-0.902579147566307));
#2697=CARTESIAN_POINT('',(85.0867659678262,12.7000000000001,-18.3323696054205));
#2698=CARTESIAN_POINT('',(45.5693348638345,12.7000000000002,-5.49237789520696));
#2699=CARTESIAN_POINT('',(82.4934155362843,12.7000000000002,-22.831167070108));
#2700=CARTESIAN_POINT('Origin',(60.4662647425757,12.7000000000001,-7.13665223247784));
#2701=CARTESIAN_POINT('',(10.1023899817279,12.7000000000002,-75.4263257814172));
#2702=CARTESIAN_POINT('Origin',(82.5541160420259,12.7,-99.0311428932582));
#2703=CARTESIAN_POINT('',(5.02238998172799,12.7000000000001,-76.5025437375311));
#2704=CARTESIAN_POINT('Origin',(1.98278330822388,12.7000000000001,-49.6273886803467));
#2705=CARTESIAN_POINT('',(5.02238998172821,12.7,-34.9514577327463));
#2706=CARTESIAN_POINT('Origin',(0.196389981728218,0.,-34.9514577327463));
#2707=CARTESIAN_POINT('',(5.02238998172821,-5.55111512312578E-14,-34.9514577327463));
#2708=CARTESIAN_POINT('',(-4.62961001827178,0.,-34.9514577327459));
#2709=CARTESIAN_POINT('Origin',(0.196389981728218,0.,-34.9514577327463));
#2710=CARTESIAN_POINT('',(5.02238998172799,1.11022302462516E-13,-76.5025437375311));
#2711=CARTESIAN_POINT('',(5.02238998172821,-5.55111512312578E-14,-34.9514577327463));
#2712=CARTESIAN_POINT('',(10.1023899817279,1.66533453693773E-13,-75.4263257814172));
#2713=CARTESIAN_POINT('Origin',(1.98278330822388,1.11022302462516E-13,-49.6273886803467));
#2714=CARTESIAN_POINT('',(82.4934155362843,1.66533453693773E-13,-22.831167070108));
#2715=CARTESIAN_POINT('Origin',(82.5541160420259,0.,-99.0311428932586));
#2716=CARTESIAN_POINT('',(85.0867659678262,0.,-18.3323696054205));
#2717=CARTESIAN_POINT('Origin',(60.4662647425757,1.11022302462516E-13,-7.13665223247784));
#2718=CARTESIAN_POINT('',(45.5693348638345,1.66533453693773E-13,-5.49237789520696));
#2719=CARTESIAN_POINT('',(45.5693348638345,1.66533453693773E-13,-5.49237789520696));
#2720=CARTESIAN_POINT('',(48.5519668935416,1.66533453693773E-13,3.6872196000739));
#2721=CARTESIAN_POINT('Origin',(47.0606508786874,1.11022302462516E-13,-0.902579147566307));
#2722=CARTESIAN_POINT('',(88.0693979975334,0.,-9.15277211014009));
#2723=CARTESIAN_POINT('',(48.5519668935416,1.66533453693773E-13,3.6872196000739));
#2724=CARTESIAN_POINT('',(88.61566022884,0.,-3.98883536926897));
#2725=CARTESIAN_POINT('Origin',(61.5703165356259,1.11022302462516E-13,-3.73873020481597));
#2726=CARTESIAN_POINT('',(60.9647489474622,1.66533453693773E-13,81.1119190693219));
#2727=CARTESIAN_POINT('Origin',(133.453989983444,0.,57.6225611805379));
#2728=CARTESIAN_POINT('',(57.4875276588944,1.11022302462516E-13,84.9685467671164));
#2729=CARTESIAN_POINT('Origin',(39.2316144081271,1.66533453693773E-13,65.0127255748485));
#2730=CARTESIAN_POINT('',(33.0644120885454,1.66533453693773E-13,51.3530120545087));
#2731=CARTESIAN_POINT('',(49.6788956291876,1.11022302462516E-13,90.6418500222421));
#2732=CARTESIAN_POINT('',(25.2557800588381,0.,57.0263153096353));
#2733=CARTESIAN_POINT('Origin',(36.3411692885802,1.66533453693773E-13,67.1127568790624));
#2734=CARTESIAN_POINT('',(-49.2861156657315,-5.55111512312578E-14,90.6418500222435));
#2735=CARTESIAN_POINT('Origin',(-35.9483893251246,1.11022302462516E-13,
67.1127568790628));
#2736=CARTESIAN_POINT('',(-24.8630000953821,1.11022302462516E-13,57.0263153096384));
#2737=CARTESIAN_POINT('',(-57.0947476954385,1.11022302462516E-13,84.9685467671164));
#2738=CARTESIAN_POINT('',(-32.6716321250895,0.,51.3530120545105));
#2739=CARTESIAN_POINT('',(-60.5719689840063,1.11022302462516E-13,81.1119190693219));
#2740=CARTESIAN_POINT('Origin',(-38.8388344446712,1.11022302462516E-13,
65.0127255748476));
#2741=CARTESIAN_POINT('',(-88.2228802653845,-5.55111512312578E-14,-3.98883536926853));
#2742=CARTESIAN_POINT('Origin',(-133.061210019987,-5.55111512312578E-14,
57.6225611805379));
#2743=CARTESIAN_POINT('',(-87.6766180340772,-5.55111512312578E-14,-9.15277211013876));
#2744=CARTESIAN_POINT('Origin',(-61.17753657217,1.11022302462516E-13,-3.73873020481819));
#2745=CARTESIAN_POINT('',(-48.1591869300858,-5.55111512312578E-14,3.68721960007434));
#2746=CARTESIAN_POINT('',(-48.1591869300858,-5.55111512312578E-14,3.68721960007434));
#2747=CARTESIAN_POINT('',(-45.1765549003784,-5.55111512312578E-14,-5.4923778952074));
#2748=CARTESIAN_POINT('Origin',(-46.6678709152318,0.,-0.902579147564531));
#2749=CARTESIAN_POINT('',(-84.6939860043709,-5.55111512312578E-14,-18.332369605421));
#2750=CARTESIAN_POINT('',(-45.1765549003784,-5.55111512312578E-14,-5.4923778952074));
#2751=CARTESIAN_POINT('',(-82.1006355728287,-5.55111512312578E-14,-22.8311670701098));
#2752=CARTESIAN_POINT('Origin',(-60.07348477912,1.11022302462516E-13,-7.13665223247828));
#2753=CARTESIAN_POINT('',(-9.70961001827242,1.11022302462516E-13,-75.4263257814172));
#2754=CARTESIAN_POINT('Origin',(-82.1613360785705,-5.55111512312578E-14,
-99.0311428932596));
#2755=CARTESIAN_POINT('',(-4.62961001827211,1.66533453693773E-13,-76.5025437375311));
#2756=CARTESIAN_POINT('Origin',(-1.59000334476844,1.11022302462516E-13,
-49.6273886803462));
#2757=CARTESIAN_POINT('',(-4.62961001827178,0.,-34.9514577327459));
#2758=CARTESIAN_POINT('Origin',(0.196389981728107,12.7,-34.9514577327463));
#2759=CARTESIAN_POINT('',(-4.62961001827178,12.7,-34.9514577327459));
#2760=CARTESIAN_POINT('',(5.02238998172821,12.7,-34.9514577327463));
#2761=CARTESIAN_POINT('Origin',(-4.62961001827178,12.7,-34.9514577327459));
#2762=CARTESIAN_POINT('',(-4.62961001827222,12.7000000000002,-76.5025437375311));
#2763=CARTESIAN_POINT('Origin',(-1.59000334476855,12.7000000000001,-49.6273886803462));
#2764=CARTESIAN_POINT('',(-9.70961001827242,12.7000000000001,-75.4263257814172));
#2765=CARTESIAN_POINT('Origin',(-82.1613360785705,12.6999999999999,-99.0311428932596));
#2766=CARTESIAN_POINT('',(-82.1006355728287,12.6999999999999,-22.8311670701098));
#2767=CARTESIAN_POINT('Origin',(-60.07348477912,12.7000000000001,-7.13665223247828));
#2768=CARTESIAN_POINT('',(-84.6939860043709,12.6999999999999,-18.332369605421));
#2769=CARTESIAN_POINT('Origin',(-45.1765549003784,12.7,-5.4923778952074));
#2770=CARTESIAN_POINT('',(-45.1765549003784,12.7,-5.4923778952074));
#2771=CARTESIAN_POINT('Origin',(-46.6678709152318,12.7,-0.902579147566751));
#2772=CARTESIAN_POINT('',(-48.1591869300858,12.7,3.68721960007434));
#2773=CARTESIAN_POINT('Origin',(-48.1591869300858,12.7,3.68721960007434));
#2774=CARTESIAN_POINT('',(-87.6766180340772,12.6999999999999,-9.15277211013876));
#2775=CARTESIAN_POINT('Origin',(-61.17753657217,12.7000000000001,-3.73873020481819));
#2776=CARTESIAN_POINT('',(-88.2228802653845,12.6999999999999,-3.98883536926853));
#2777=CARTESIAN_POINT('Origin',(-133.061210019987,12.7,57.6225611805379));
#2778=CARTESIAN_POINT('',(-60.5719689840063,12.7000000000001,81.1119190693219));
#2779=CARTESIAN_POINT('Origin',(-38.8388344446712,12.7000000000001,65.0127255748467));
#2780=CARTESIAN_POINT('',(-57.0947476954385,12.7000000000001,84.9685467671164));
#2781=CARTESIAN_POINT('Origin',(-32.6716321250896,12.7,51.35301205451));
#2782=CARTESIAN_POINT('Origin',(-24.8630000953821,12.7000000000001,57.0263153096384));
#2783=CARTESIAN_POINT('',(-49.2861156657315,12.7,90.6418500222435));
#2784=CARTESIAN_POINT('Origin',(-35.9483893251246,12.7000000000001,67.1127568790628));
#2785=CARTESIAN_POINT('Origin',(36.3411692885806,12.7000000000002,67.1127568790633));
#2786=CARTESIAN_POINT('',(49.6788956291876,12.7000000000001,90.6418500222421));
#2787=CARTESIAN_POINT('Origin',(25.2557800588381,12.7,57.0263153096353));
#2788=CARTESIAN_POINT('Origin',(33.0644120885452,12.7000000000002,51.3530120545092));
#2789=CARTESIAN_POINT('',(57.4875276588944,12.7000000000001,84.9685467671164));
#2790=CARTESIAN_POINT('Origin',(39.2316144081271,12.7000000000002,65.0127255748485));
#2791=CARTESIAN_POINT('',(60.964748947462,12.7000000000002,81.1119190693224));
#2792=CARTESIAN_POINT('Origin',(133.453989983443,12.7,57.6225611805374));
#2793=CARTESIAN_POINT('',(88.61566022884,12.7,-3.98883536926897));
#2794=CARTESIAN_POINT('Origin',(61.5703165356259,12.7000000000001,-3.73873020481819));
#2795=CARTESIAN_POINT('',(88.0693979975334,12.7,-9.15277211014009));
#2796=CARTESIAN_POINT('Origin',(48.5519668935416,12.7000000000002,3.6872196000739));
#2797=CARTESIAN_POINT('',(48.5519668935416,12.7000000000002,3.6872196000739));
#2798=CARTESIAN_POINT('Origin',(47.0606508786874,12.7000000000001,-0.902579147566307));
#2799=CARTESIAN_POINT('',(45.5693348638345,12.7000000000002,-5.49237789520696));
#2800=CARTESIAN_POINT('Origin',(45.5693348638345,12.7000000000002,-5.49237789520696));
#2801=CARTESIAN_POINT('',(85.0867659678262,12.7000000000001,-18.3323696054205));
#2802=CARTESIAN_POINT('Origin',(60.4662647425757,12.7000000000001,-7.13665223247784));
#2803=CARTESIAN_POINT('',(82.4934155362843,12.7000000000002,-22.831167070108));
#2804=CARTESIAN_POINT('Origin',(82.5541160420259,12.7,-99.0311428932582));
#2805=CARTESIAN_POINT('',(10.1023899817279,12.7000000000002,-75.4263257814172));
#2806=CARTESIAN_POINT('Origin',(1.98278330822388,12.7000000000001,-49.6273886803467));
#2807=CARTESIAN_POINT('',(5.02238998172799,12.7000000000001,-76.5025437375311));
#2808=CARTESIAN_POINT('Origin',(5.02238998172821,12.7,-34.9514577327463));
#2809=CARTESIAN_POINT('Origin',(0.196389981728107,9.52499999999995,14.3245422672531));
#2810=CARTESIAN_POINT('',(0.,0.,0.));
#2811=CARTESIAN_POINT('Origin',(0.,45.,0.));
#2812=CARTESIAN_POINT('',(-1.088711004442E-15,0.,8.89));
#2813=CARTESIAN_POINT('Origin',(0.,0.,0.));
#2814=CARTESIAN_POINT('',(-1.088711004442E-15,45.,8.89));
#2815=CARTESIAN_POINT('',(-1.088711004442E-15,45.,8.89));
#2816=CARTESIAN_POINT('Origin',(0.,45.,0.));
#2817=CARTESIAN_POINT('Origin',(0.,45.,0.));
#2818=CARTESIAN_POINT('Origin',(0.,0.,0.));
#2819=CARTESIAN_POINT('',(0.,0.,0.));
#2820=CARTESIAN_POINT('',(-143.227160903632,30.,-1545.5527252068));
#2821=CARTESIAN_POINT('',(-210.432495197589,47.0000000000002,-2131.93341554535));
#2822=CARTESIAN_POINT('',(107.996822771948,47.,-2150.79718544047));
#2823=CARTESIAN_POINT('',(88.8313006293733,64.0000000000002,-2238.01489586509));
#2824=CARTESIAN_POINT('',(84.5196618610051,36.7000000000002,-2224.35323962134));
#2825=UNCERTAINTY_MEASURE_WITH_UNIT(LENGTH_MEASURE(0.01),#2841,
'DISTANCE_ACCURACY_VALUE',
'Maximum model space distance between geometric entities at asserted c
onnectivities');
#2826=UNCERTAINTY_MEASURE_WITH_UNIT(LENGTH_MEASURE(0.01),#2841,
'DISTANCE_ACCURACY_VALUE',
'Maximum model space distance between geometric entities at asserted c
onnectivities');
#2827=UNCERTAINTY_MEASURE_WITH_UNIT(LENGTH_MEASURE(0.01),#2841,
'DISTANCE_ACCURACY_VALUE',
'Maximum model space distance between geometric entities at asserted c
onnectivities');
#2828=UNCERTAINTY_MEASURE_WITH_UNIT(LENGTH_MEASURE(0.01),#2841,
'DISTANCE_ACCURACY_VALUE',
'Maximum model space distance between geometric entities at asserted c
onnectivities');
#2829=UNCERTAINTY_MEASURE_WITH_UNIT(LENGTH_MEASURE(0.01),#2841,
'DISTANCE_ACCURACY_VALUE',
'Maximum model space distance between geometric entities at asserted c
onnectivities');
#2830=UNCERTAINTY_MEASURE_WITH_UNIT(LENGTH_MEASURE(0.01),#2841,
'DISTANCE_ACCURACY_VALUE',
'Maximum model space distance between geometric entities at asserted c
onnectivities');
#2831=UNCERTAINTY_MEASURE_WITH_UNIT(LENGTH_MEASURE(0.01),#2841,
'DISTANCE_ACCURACY_VALUE',
'Maximum model space distance between geometric entities at asserted c
onnectivities');
#2832=UNCERTAINTY_MEASURE_WITH_UNIT(LENGTH_MEASURE(0.01),#2841,
'DISTANCE_ACCURACY_VALUE',
'Maximum model space distance between geometric entities at asserted c
onnectivities');
#2833=(
GEOMETRIC_REPRESENTATION_CONTEXT(3)
GLOBAL_UNCERTAINTY_ASSIGNED_CONTEXT((#2825))
GLOBAL_UNIT_ASSIGNED_CONTEXT((#2841,#2843,#2844))
REPRESENTATION_CONTEXT('','3D')
);
#2834=(
GEOMETRIC_REPRESENTATION_CONTEXT(3)
GLOBAL_UNCERTAINTY_ASSIGNED_CONTEXT((#2826))
GLOBAL_UNIT_ASSIGNED_CONTEXT((#2841,#2843,#2844))
REPRESENTATION_CONTEXT('','3D')
);
#2835=(
GEOMETRIC_REPRESENTATION_CONTEXT(3)
GLOBAL_UNCERTAINTY_ASSIGNED_CONTEXT((#2827))
GLOBAL_UNIT_ASSIGNED_CONTEXT((#2841,#2843,#2844))
REPRESENTATION_CONTEXT('','3D')
);
#2836=(
GEOMETRIC_REPRESENTATION_CONTEXT(3)
GLOBAL_UNCERTAINTY_ASSIGNED_CONTEXT((#2828))
GLOBAL_UNIT_ASSIGNED_CONTEXT((#2841,#2843,#2844))
REPRESENTATION_CONTEXT('','3D')
);
#2837=(
GEOMETRIC_REPRESENTATION_CONTEXT(3)
GLOBAL_UNCERTAINTY_ASSIGNED_CONTEXT((#2829))
GLOBAL_UNIT_ASSIGNED_CONTEXT((#2841,#2843,#2844))
REPRESENTATION_CONTEXT('','3D')
);
#2838=(
GEOMETRIC_REPRESENTATION_CONTEXT(3)
GLOBAL_UNCERTAINTY_ASSIGNED_CONTEXT((#2830))
GLOBAL_UNIT_ASSIGNED_CONTEXT((#2841,#2843,#2844))
REPRESENTATION_CONTEXT('','3D')
);
#2839=(
GEOMETRIC_REPRESENTATION_CONTEXT(3)
GLOBAL_UNCERTAINTY_ASSIGNED_CONTEXT((#2831))
GLOBAL_UNIT_ASSIGNED_CONTEXT((#2841,#2843,#2844))
REPRESENTATION_CONTEXT('','3D')
);
#2840=(
GEOMETRIC_REPRESENTATION_CONTEXT(3)
GLOBAL_UNCERTAINTY_ASSIGNED_CONTEXT((#2832))
GLOBAL_UNIT_ASSIGNED_CONTEXT((#2841,#2843,#2844))
REPRESENTATION_CONTEXT('','3D')
);
#2841=(
LENGTH_UNIT()
NAMED_UNIT(*)
SI_UNIT(.MILLI.,.METRE.)
);
#2842=(
LENGTH_UNIT()
NAMED_UNIT(*)
SI_UNIT($,.METRE.)
);
#2843=(
NAMED_UNIT(*)
PLANE_ANGLE_UNIT()
SI_UNIT($,.RADIAN.)
);
#2844=(
NAMED_UNIT(*)
SI_UNIT($,.STERADIAN.)
SOLID_ANGLE_UNIT()
);
#2845=SHAPE_DEFINITION_REPRESENTATION(#2852,#2865);
#2846=SHAPE_DEFINITION_REPRESENTATION(#2853,#2866);
#2847=SHAPE_DEFINITION_REPRESENTATION(#2854,#2867);
#2848=SHAPE_DEFINITION_REPRESENTATION(#2855,#2868);
#2849=SHAPE_DEFINITION_REPRESENTATION(#2856,#2869);
#2850=SHAPE_DEFINITION_REPRESENTATION(#2857,#2870);
#2851=SHAPE_DEFINITION_REPRESENTATION(#2858,#2871);
#2852=PRODUCT_DEFINITION_SHAPE('',$,#2873);
#2853=PRODUCT_DEFINITION_SHAPE('',$,#2874);
#2854=PRODUCT_DEFINITION_SHAPE('',$,#2875);
#2855=PRODUCT_DEFINITION_SHAPE('',$,#2876);
#2856=PRODUCT_DEFINITION_SHAPE('',$,#2877);
#2857=PRODUCT_DEFINITION_SHAPE('',$,#2878);
#2858=PRODUCT_DEFINITION_SHAPE('',$,#2879);
#2859=PRODUCT_DEFINITION_SHAPE($,$,#29);
#2860=PRODUCT_DEFINITION_SHAPE($,$,#30);
#2861=PRODUCT_DEFINITION_SHAPE($,$,#31);
#2862=PRODUCT_DEFINITION_SHAPE($,$,#32);
#2863=PRODUCT_DEFINITION_SHAPE($,$,#33);
#2864=PRODUCT_DEFINITION_SHAPE($,$,#34);
#2865=SHAPE_REPRESENTATION('',(#1620,#1835,#1836,#1837,#1838,#1839,#1840),
#2833);
#2866=SHAPE_REPRESENTATION('',(#1621),#2834);
#2867=SHAPE_REPRESENTATION('',(#1696),#2835);
#2868=SHAPE_REPRESENTATION('',(#1709),#2836);
#2869=SHAPE_REPRESENTATION('',(#1743),#2837);
#2870=SHAPE_REPRESENTATION('',(#1749),#2838);
#2871=SHAPE_REPRESENTATION('',(#1829),#2839);
#2872=PRODUCT_DEFINITION_CONTEXT('part definition',#2895,'design');
#2873=PRODUCT_DEFINITION('Geneva Drive Rotary Indexing Table Assembly',
'MAS-609',#2880,#2872);
#2874=PRODUCT_DEFINITION('BASE PLATE','BASE PLATE',#2881,#2872);
#2875=PRODUCT_DEFINITION('ROUND DISC','ROUND DISC',#2882,#2872);
#2876=PRODUCT_DEFINITION('SMALL DISC','SMALL DISC',#2883,#2872);
#2877=PRODUCT_DEFINITION('Pin','PIN',#2884,#2872);
#2878=PRODUCT_DEFINITION('Geneva Wheel','Geneva Wheel',#2885,#2872);
#2879=PRODUCT_DEFINITION('Shaft','SHAFT',#2886,#2872);
#2880=PRODUCT_DEFINITION_FORMATION('',$,#2897);
#2881=PRODUCT_DEFINITION_FORMATION('',$,#2898);
#2882=PRODUCT_DEFINITION_FORMATION('',$,#2899);
#2883=PRODUCT_DEFINITION_FORMATION('',$,#2900);
#2884=PRODUCT_DEFINITION_FORMATION('',$,#2901);
#2885=PRODUCT_DEFINITION_FORMATION('',$,#2902);
#2886=PRODUCT_DEFINITION_FORMATION('',$,#2903);
#2887=PRODUCT_RELATED_PRODUCT_CATEGORY(
'MAS-609',
'MAS-609',(#2897));
#2888=PRODUCT_RELATED_PRODUCT_CATEGORY('BASE PLATE','BASE PLATE',(#2898));
#2889=PRODUCT_RELATED_PRODUCT_CATEGORY('ROUND DISC','ROUND DISC',(#2899));
#2890=PRODUCT_RELATED_PRODUCT_CATEGORY('SMALL DISC','SMALL DISC',(#2900));
#2891=PRODUCT_RELATED_PRODUCT_CATEGORY('PIN','PIN',(#2901));
#2892=PRODUCT_RELATED_PRODUCT_CATEGORY('Geneva Wheel','Geneva Wheel',(#2902));
#2893=PRODUCT_RELATED_PRODUCT_CATEGORY('SHAFT','SHAFT',(#2903));
#2894=APPLICATION_PROTOCOL_DEFINITION('international standard',
'automotive_design',2009,#2895);
#2895=APPLICATION_CONTEXT(
'Core Data for Automotive Mechanical Design Process');
#2896=PRODUCT_CONTEXT('part definition',#2895,'mechanical');
#2897=PRODUCT('Geneva Drive Rotary Indexing Table Assembly',
'MAS-609','STEP AP214',(#2896));
#2898=PRODUCT('BASE PLATE','BASE PLATE',$,(#2896));
#2899=PRODUCT('ROUND DISC','ROUND DISC',$,(#2896));
#2900=PRODUCT('SMALL DISC','SMALL DISC',$,(#2896));
#2901=PRODUCT('Pin','PIN',$,(#2896));
#2902=PRODUCT('Geneva Wheel','Geneva Wheel',$,(#2896));
#2903=PRODUCT('Shaft','SHAFT',$,(#2896));
#2904=PRESENTATION_STYLE_ASSIGNMENT((#2906));
#2905=PRESENTATION_STYLE_ASSIGNMENT((#2907));
#2906=SURFACE_STYLE_USAGE(.BOTH.,#2908);
#2907=SURFACE_STYLE_USAGE(.BOTH.,#2909);
#2908=SURFACE_SIDE_STYLE('',(#2910));
#2909=SURFACE_SIDE_STYLE('',(#2911));
#2910=SURFACE_STYLE_FILL_AREA(#2912);
#2911=SURFACE_STYLE_FILL_AREA(#2913);
#2912=FILL_AREA_STYLE('Steel - Satin',(#2914));
#2913=FILL_AREA_STYLE('Opaque(202,209,238)',(#2915));
#2914=FILL_AREA_STYLE_COLOUR('Steel - Satin',#2916);
#2915=FILL_AREA_STYLE_COLOUR('Opaque(202,209,238)',#2917);
#2916=COLOUR_RGB('Steel - Satin', 0.66274510, 0.83137255, 0.94901961);
#2917=COLOUR_RGB('Opaque(202,209,238)', 0.66274510, 0.83137255, 0.94901961);
ENDSEC;
END-ISO-10303-21;
